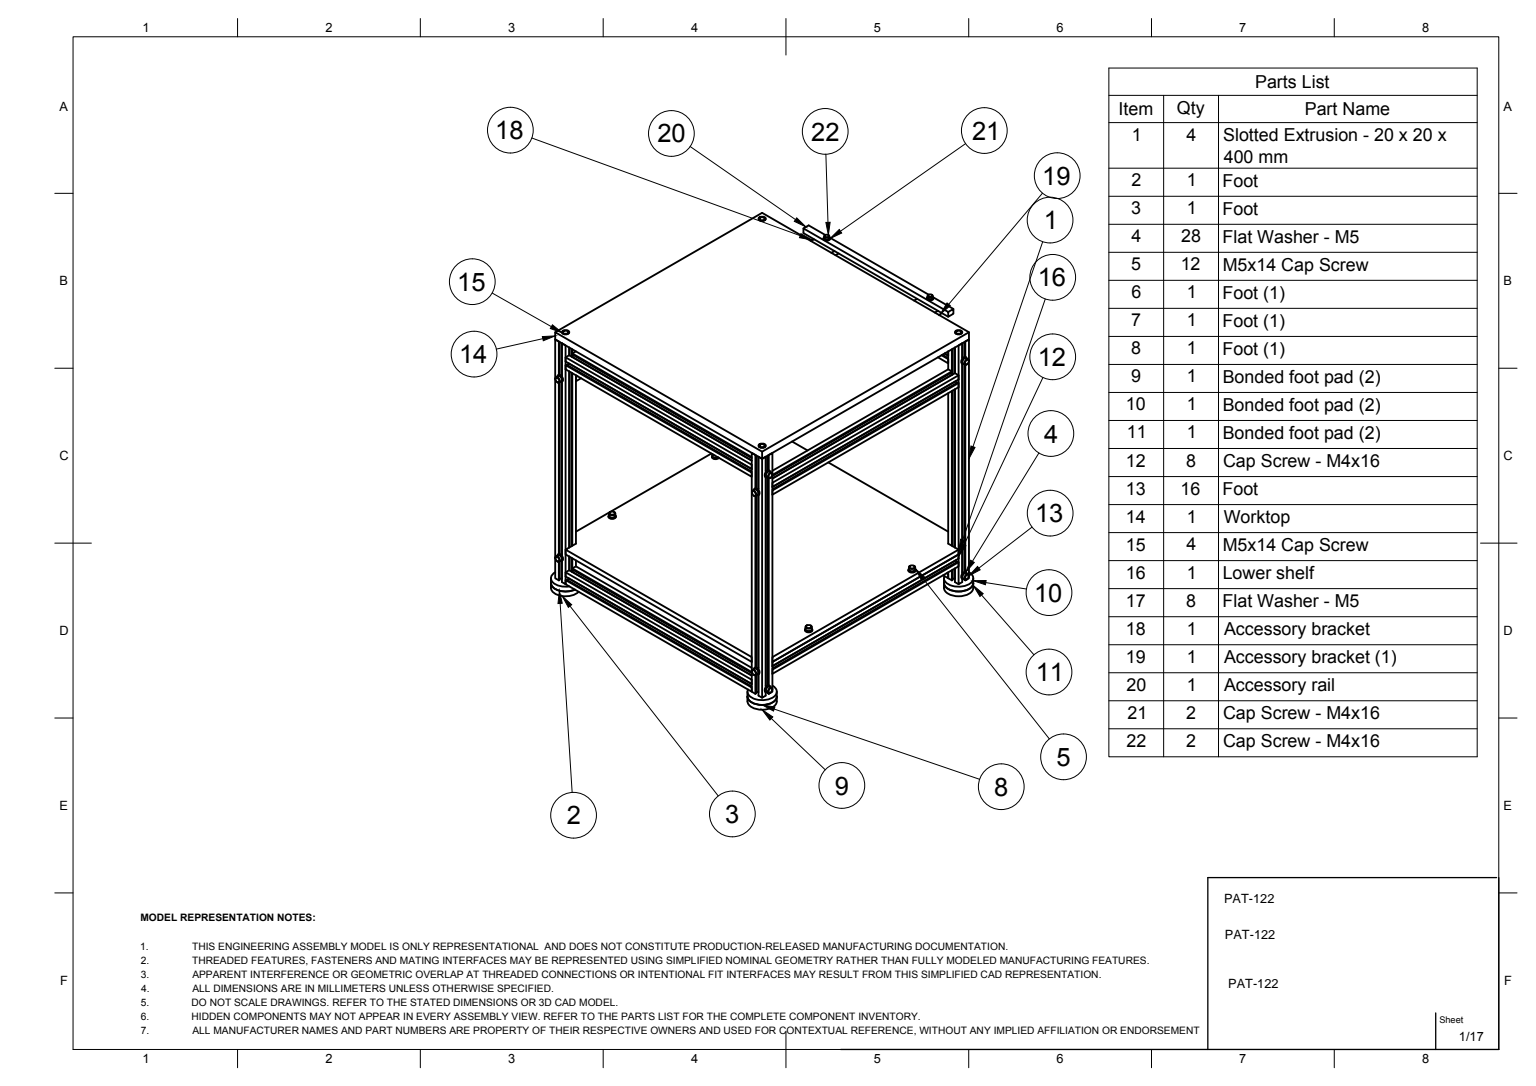
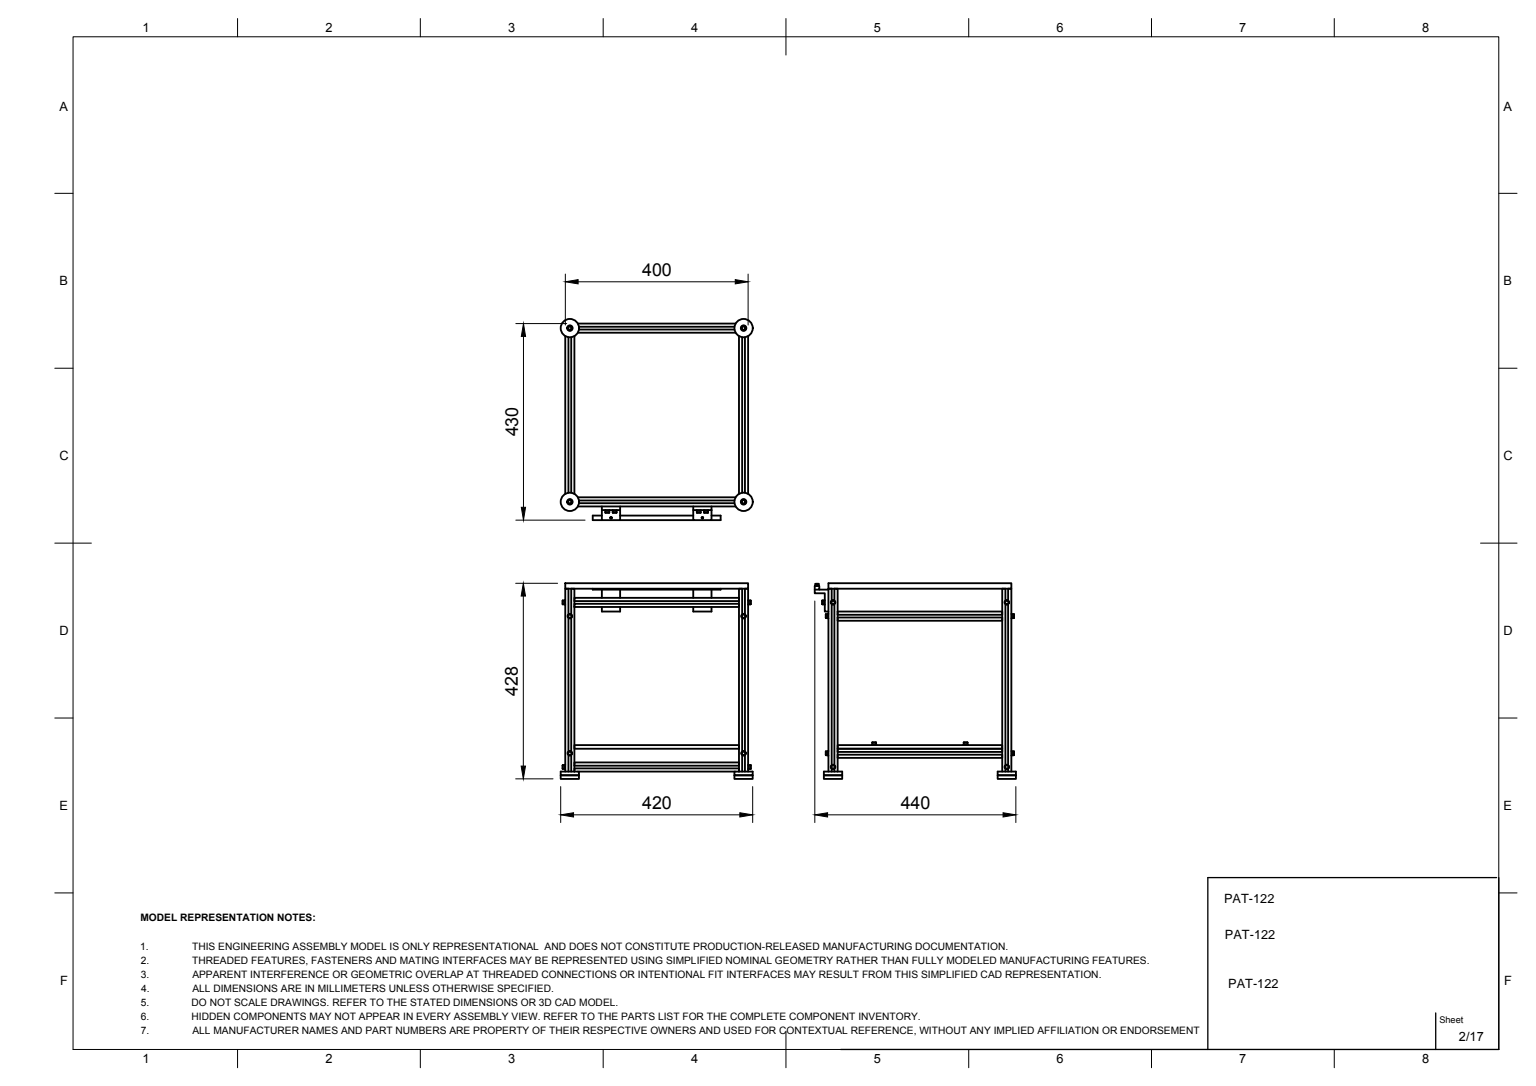
ISO-10303-21;
HEADER;
/* Generated by software containing ST-Developer
 * from STEP Tools, Inc. (www.steptools.com) 
 */

FILE_DESCRIPTION(
/* description */ ('PAT-122'),
/* implementation_level */ '2;1');

FILE_NAME(
/* name */ 'PAT-122',
/* time_stamp */ '2026-10-29T20:20:12-07:00',
/* author */ (''),
/* organization */ (''),
/* preprocessor_version */ 'ST-DEVELOPER v20.2',
/* originating_system */ 'Autodesk Translation Framework v15.17.0.0',
/* authorisation */ '');

FILE_SCHEMA (('AUTOMOTIVE_DESIGN { 1 0 10303 214 3 1 1 }'));
ENDSEC;

DATA;
#10=MECHANICAL_DESIGN_GEOMETRIC_PRESENTATION_REPRESENTATION('',(#491,#492,
#493,#494,#495,#496,#497,#498,#499,#500,#501,#502,#503,#504,#505,#506,#507,
#508,#509,#510,#511,#512),#10019);
#11=ITEM_DEFINED_TRANSFORMATION($,$,#5883,#6329);
#12=ITEM_DEFINED_TRANSFORMATION($,$,#5892,#6330);
#13=ITEM_DEFINED_TRANSFORMATION($,$,#5901,#6331);
#14=ITEM_DEFINED_TRANSFORMATION($,$,#5910,#6332);
#15=ITEM_DEFINED_TRANSFORMATION($,$,#5919,#6333);
#16=ITEM_DEFINED_TRANSFORMATION($,$,#5928,#6334);
#17=ITEM_DEFINED_TRANSFORMATION($,$,#5937,#6335);
#18=ITEM_DEFINED_TRANSFORMATION($,$,#5946,#6336);
#19=ITEM_DEFINED_TRANSFORMATION($,$,#5955,#6337);
#20=ITEM_DEFINED_TRANSFORMATION($,$,#5990,#6338);
#21=ITEM_DEFINED_TRANSFORMATION($,$,#6017,#6339);
#22=ITEM_DEFINED_TRANSFORMATION($,$,#6035,#6340);
#23=ITEM_DEFINED_TRANSFORMATION($,$,#6053,#6341);
#24=ITEM_DEFINED_TRANSFORMATION($,$,#6066,#6342);
#25=ITEM_DEFINED_TRANSFORMATION($,$,#6257,#6343);
#26=ITEM_DEFINED_TRANSFORMATION($,$,#6268,#6344);
#27=ITEM_DEFINED_TRANSFORMATION($,$,#6066,#6345);
#28=ITEM_DEFINED_TRANSFORMATION($,$,#6257,#6346);
#29=ITEM_DEFINED_TRANSFORMATION($,$,#6268,#6347);
#30=ITEM_DEFINED_TRANSFORMATION($,$,#6066,#6348);
#31=ITEM_DEFINED_TRANSFORMATION($,$,#6257,#6349);
#32=ITEM_DEFINED_TRANSFORMATION($,$,#6268,#6350);
#33=ITEM_DEFINED_TRANSFORMATION($,$,#6066,#6351);
#34=ITEM_DEFINED_TRANSFORMATION($,$,#6257,#6352);
#35=ITEM_DEFINED_TRANSFORMATION($,$,#6268,#6353);
#36=ITEM_DEFINED_TRANSFORMATION($,$,#6132,#6354);
#37=ITEM_DEFINED_TRANSFORMATION($,$,#6257,#6355);
#38=ITEM_DEFINED_TRANSFORMATION($,$,#6182,#6356);
#39=ITEM_DEFINED_TRANSFORMATION($,$,#6257,#6357);
#40=ITEM_DEFINED_TRANSFORMATION($,$,#6182,#6358);
#41=ITEM_DEFINED_TRANSFORMATION($,$,#6132,#6359);
#42=ITEM_DEFINED_TRANSFORMATION($,$,#6257,#6360);
#43=ITEM_DEFINED_TRANSFORMATION($,$,#6182,#6361);
#44=ITEM_DEFINED_TRANSFORMATION($,$,#6257,#6362);
#45=ITEM_DEFINED_TRANSFORMATION($,$,#6182,#6363);
#46=ITEM_DEFINED_TRANSFORMATION($,$,#6132,#6364);
#47=ITEM_DEFINED_TRANSFORMATION($,$,#6257,#6365);
#48=ITEM_DEFINED_TRANSFORMATION($,$,#6182,#6366);
#49=ITEM_DEFINED_TRANSFORMATION($,$,#6257,#6367);
#50=ITEM_DEFINED_TRANSFORMATION($,$,#6182,#6368);
#51=ITEM_DEFINED_TRANSFORMATION($,$,#6132,#6369);
#52=ITEM_DEFINED_TRANSFORMATION($,$,#6257,#6370);
#53=ITEM_DEFINED_TRANSFORMATION($,$,#6182,#6371);
#54=ITEM_DEFINED_TRANSFORMATION($,$,#6257,#6372);
#55=ITEM_DEFINED_TRANSFORMATION($,$,#6182,#6373);
#56=ITEM_DEFINED_TRANSFORMATION($,$,#6132,#6374);
#57=ITEM_DEFINED_TRANSFORMATION($,$,#6257,#6375);
#58=ITEM_DEFINED_TRANSFORMATION($,$,#6182,#6376);
#59=ITEM_DEFINED_TRANSFORMATION($,$,#6257,#6377);
#60=ITEM_DEFINED_TRANSFORMATION($,$,#6182,#6378);
#61=ITEM_DEFINED_TRANSFORMATION($,$,#6132,#6379);
#62=ITEM_DEFINED_TRANSFORMATION($,$,#6257,#6380);
#63=ITEM_DEFINED_TRANSFORMATION($,$,#6182,#6381);
#64=ITEM_DEFINED_TRANSFORMATION($,$,#6257,#6382);
#65=ITEM_DEFINED_TRANSFORMATION($,$,#6182,#6383);
#66=ITEM_DEFINED_TRANSFORMATION($,$,#6132,#6384);
#67=ITEM_DEFINED_TRANSFORMATION($,$,#6257,#6385);
#68=ITEM_DEFINED_TRANSFORMATION($,$,#6182,#6386);
#69=ITEM_DEFINED_TRANSFORMATION($,$,#6257,#6387);
#70=ITEM_DEFINED_TRANSFORMATION($,$,#6182,#6388);
#71=ITEM_DEFINED_TRANSFORMATION($,$,#6132,#6389);
#72=ITEM_DEFINED_TRANSFORMATION($,$,#6257,#6390);
#73=ITEM_DEFINED_TRANSFORMATION($,$,#6182,#6391);
#74=ITEM_DEFINED_TRANSFORMATION($,$,#6257,#6392);
#75=ITEM_DEFINED_TRANSFORMATION($,$,#6182,#6393);
#76=ITEM_DEFINED_TRANSFORMATION($,$,#6210,#6394);
#77=ITEM_DEFINED_TRANSFORMATION($,$,#6210,#6395);
#78=ITEM_DEFINED_TRANSFORMATION($,$,#6210,#6396);
#79=ITEM_DEFINED_TRANSFORMATION($,$,#6210,#6397);
#80=ITEM_DEFINED_TRANSFORMATION($,$,#6236,#6398);
#81=ITEM_DEFINED_TRANSFORMATION($,$,#6257,#6399);
#82=ITEM_DEFINED_TRANSFORMATION($,$,#6268,#6400);
#83=ITEM_DEFINED_TRANSFORMATION($,$,#6236,#6401);
#84=ITEM_DEFINED_TRANSFORMATION($,$,#6257,#6402);
#85=ITEM_DEFINED_TRANSFORMATION($,$,#6268,#6403);
#86=ITEM_DEFINED_TRANSFORMATION($,$,#6236,#6404);
#87=ITEM_DEFINED_TRANSFORMATION($,$,#6257,#6405);
#88=ITEM_DEFINED_TRANSFORMATION($,$,#6268,#6406);
#89=ITEM_DEFINED_TRANSFORMATION($,$,#6236,#6407);
#90=ITEM_DEFINED_TRANSFORMATION($,$,#6257,#6408);
#91=ITEM_DEFINED_TRANSFORMATION($,$,#6268,#6409);
#92=ITEM_DEFINED_TRANSFORMATION($,$,#6236,#6410);
#93=ITEM_DEFINED_TRANSFORMATION($,$,#6257,#6411);
#94=ITEM_DEFINED_TRANSFORMATION($,$,#6268,#6412);
#95=ITEM_DEFINED_TRANSFORMATION($,$,#6236,#6413);
#96=ITEM_DEFINED_TRANSFORMATION($,$,#6257,#6414);
#97=ITEM_DEFINED_TRANSFORMATION($,$,#6268,#6415);
#98=ITEM_DEFINED_TRANSFORMATION($,$,#6236,#6416);
#99=ITEM_DEFINED_TRANSFORMATION($,$,#6257,#6417);
#100=ITEM_DEFINED_TRANSFORMATION($,$,#6268,#6418);
#101=ITEM_DEFINED_TRANSFORMATION($,$,#6236,#6419);
#102=ITEM_DEFINED_TRANSFORMATION($,$,#6257,#6420);
#103=ITEM_DEFINED_TRANSFORMATION($,$,#6268,#6421);
#104=ITEM_DEFINED_TRANSFORMATION($,$,#6292,#6422);
#105=ITEM_DEFINED_TRANSFORMATION($,$,#6303,#6423);
#106=ITEM_DEFINED_TRANSFORMATION($,$,#6292,#6424);
#107=ITEM_DEFINED_TRANSFORMATION($,$,#6303,#6425);
#108=(
REPRESENTATION_RELATIONSHIP($,$,#10168,#10167)
REPRESENTATION_RELATIONSHIP_WITH_TRANSFORMATION(#11)
SHAPE_REPRESENTATION_RELATIONSHIP()
);
#109=(
REPRESENTATION_RELATIONSHIP($,$,#10169,#10167)
REPRESENTATION_RELATIONSHIP_WITH_TRANSFORMATION(#12)
SHAPE_REPRESENTATION_RELATIONSHIP()
);
#110=(
REPRESENTATION_RELATIONSHIP($,$,#10170,#10167)
REPRESENTATION_RELATIONSHIP_WITH_TRANSFORMATION(#13)
SHAPE_REPRESENTATION_RELATIONSHIP()
);
#111=(
REPRESENTATION_RELATIONSHIP($,$,#10171,#10167)
REPRESENTATION_RELATIONSHIP_WITH_TRANSFORMATION(#14)
SHAPE_REPRESENTATION_RELATIONSHIP()
);
#112=(
REPRESENTATION_RELATIONSHIP($,$,#10172,#10167)
REPRESENTATION_RELATIONSHIP_WITH_TRANSFORMATION(#15)
SHAPE_REPRESENTATION_RELATIONSHIP()
);
#113=(
REPRESENTATION_RELATIONSHIP($,$,#10173,#10167)
REPRESENTATION_RELATIONSHIP_WITH_TRANSFORMATION(#16)
SHAPE_REPRESENTATION_RELATIONSHIP()
);
#114=(
REPRESENTATION_RELATIONSHIP($,$,#10174,#10167)
REPRESENTATION_RELATIONSHIP_WITH_TRANSFORMATION(#17)
SHAPE_REPRESENTATION_RELATIONSHIP()
);
#115=(
REPRESENTATION_RELATIONSHIP($,$,#10175,#10167)
REPRESENTATION_RELATIONSHIP_WITH_TRANSFORMATION(#18)
SHAPE_REPRESENTATION_RELATIONSHIP()
);
#116=(
REPRESENTATION_RELATIONSHIP($,$,#10176,#10167)
REPRESENTATION_RELATIONSHIP_WITH_TRANSFORMATION(#19)
SHAPE_REPRESENTATION_RELATIONSHIP()
);
#117=(
REPRESENTATION_RELATIONSHIP($,$,#10177,#10167)
REPRESENTATION_RELATIONSHIP_WITH_TRANSFORMATION(#20)
SHAPE_REPRESENTATION_RELATIONSHIP()
);
#118=(
REPRESENTATION_RELATIONSHIP($,$,#10178,#10167)
REPRESENTATION_RELATIONSHIP_WITH_TRANSFORMATION(#21)
SHAPE_REPRESENTATION_RELATIONSHIP()
);
#119=(
REPRESENTATION_RELATIONSHIP($,$,#10179,#10167)
REPRESENTATION_RELATIONSHIP_WITH_TRANSFORMATION(#22)
SHAPE_REPRESENTATION_RELATIONSHIP()
);
#120=(
REPRESENTATION_RELATIONSHIP($,$,#10180,#10167)
REPRESENTATION_RELATIONSHIP_WITH_TRANSFORMATION(#23)
SHAPE_REPRESENTATION_RELATIONSHIP()
);
#121=(
REPRESENTATION_RELATIONSHIP($,$,#10181,#10167)
REPRESENTATION_RELATIONSHIP_WITH_TRANSFORMATION(#24)
SHAPE_REPRESENTATION_RELATIONSHIP()
);
#122=(
REPRESENTATION_RELATIONSHIP($,$,#10186,#10167)
REPRESENTATION_RELATIONSHIP_WITH_TRANSFORMATION(#25)
SHAPE_REPRESENTATION_RELATIONSHIP()
);
#123=(
REPRESENTATION_RELATIONSHIP($,$,#10187,#10167)
REPRESENTATION_RELATIONSHIP_WITH_TRANSFORMATION(#26)
SHAPE_REPRESENTATION_RELATIONSHIP()
);
#124=(
REPRESENTATION_RELATIONSHIP($,$,#10181,#10167)
REPRESENTATION_RELATIONSHIP_WITH_TRANSFORMATION(#27)
SHAPE_REPRESENTATION_RELATIONSHIP()
);
#125=(
REPRESENTATION_RELATIONSHIP($,$,#10186,#10167)
REPRESENTATION_RELATIONSHIP_WITH_TRANSFORMATION(#28)
SHAPE_REPRESENTATION_RELATIONSHIP()
);
#126=(
REPRESENTATION_RELATIONSHIP($,$,#10187,#10167)
REPRESENTATION_RELATIONSHIP_WITH_TRANSFORMATION(#29)
SHAPE_REPRESENTATION_RELATIONSHIP()
);
#127=(
REPRESENTATION_RELATIONSHIP($,$,#10181,#10167)
REPRESENTATION_RELATIONSHIP_WITH_TRANSFORMATION(#30)
SHAPE_REPRESENTATION_RELATIONSHIP()
);
#128=(
REPRESENTATION_RELATIONSHIP($,$,#10186,#10167)
REPRESENTATION_RELATIONSHIP_WITH_TRANSFORMATION(#31)
SHAPE_REPRESENTATION_RELATIONSHIP()
);
#129=(
REPRESENTATION_RELATIONSHIP($,$,#10187,#10167)
REPRESENTATION_RELATIONSHIP_WITH_TRANSFORMATION(#32)
SHAPE_REPRESENTATION_RELATIONSHIP()
);
#130=(
REPRESENTATION_RELATIONSHIP($,$,#10181,#10167)
REPRESENTATION_RELATIONSHIP_WITH_TRANSFORMATION(#33)
SHAPE_REPRESENTATION_RELATIONSHIP()
);
#131=(
REPRESENTATION_RELATIONSHIP($,$,#10186,#10167)
REPRESENTATION_RELATIONSHIP_WITH_TRANSFORMATION(#34)
SHAPE_REPRESENTATION_RELATIONSHIP()
);
#132=(
REPRESENTATION_RELATIONSHIP($,$,#10187,#10167)
REPRESENTATION_RELATIONSHIP_WITH_TRANSFORMATION(#35)
SHAPE_REPRESENTATION_RELATIONSHIP()
);
#133=(
REPRESENTATION_RELATIONSHIP($,$,#10182,#10167)
REPRESENTATION_RELATIONSHIP_WITH_TRANSFORMATION(#36)
SHAPE_REPRESENTATION_RELATIONSHIP()
);
#134=(
REPRESENTATION_RELATIONSHIP($,$,#10186,#10167)
REPRESENTATION_RELATIONSHIP_WITH_TRANSFORMATION(#37)
SHAPE_REPRESENTATION_RELATIONSHIP()
);
#135=(
REPRESENTATION_RELATIONSHIP($,$,#10183,#10167)
REPRESENTATION_RELATIONSHIP_WITH_TRANSFORMATION(#38)
SHAPE_REPRESENTATION_RELATIONSHIP()
);
#136=(
REPRESENTATION_RELATIONSHIP($,$,#10186,#10167)
REPRESENTATION_RELATIONSHIP_WITH_TRANSFORMATION(#39)
SHAPE_REPRESENTATION_RELATIONSHIP()
);
#137=(
REPRESENTATION_RELATIONSHIP($,$,#10183,#10167)
REPRESENTATION_RELATIONSHIP_WITH_TRANSFORMATION(#40)
SHAPE_REPRESENTATION_RELATIONSHIP()
);
#138=(
REPRESENTATION_RELATIONSHIP($,$,#10182,#10167)
REPRESENTATION_RELATIONSHIP_WITH_TRANSFORMATION(#41)
SHAPE_REPRESENTATION_RELATIONSHIP()
);
#139=(
REPRESENTATION_RELATIONSHIP($,$,#10186,#10167)
REPRESENTATION_RELATIONSHIP_WITH_TRANSFORMATION(#42)
SHAPE_REPRESENTATION_RELATIONSHIP()
);
#140=(
REPRESENTATION_RELATIONSHIP($,$,#10183,#10167)
REPRESENTATION_RELATIONSHIP_WITH_TRANSFORMATION(#43)
SHAPE_REPRESENTATION_RELATIONSHIP()
);
#141=(
REPRESENTATION_RELATIONSHIP($,$,#10186,#10167)
REPRESENTATION_RELATIONSHIP_WITH_TRANSFORMATION(#44)
SHAPE_REPRESENTATION_RELATIONSHIP()
);
#142=(
REPRESENTATION_RELATIONSHIP($,$,#10183,#10167)
REPRESENTATION_RELATIONSHIP_WITH_TRANSFORMATION(#45)
SHAPE_REPRESENTATION_RELATIONSHIP()
);
#143=(
REPRESENTATION_RELATIONSHIP($,$,#10182,#10167)
REPRESENTATION_RELATIONSHIP_WITH_TRANSFORMATION(#46)
SHAPE_REPRESENTATION_RELATIONSHIP()
);
#144=(
REPRESENTATION_RELATIONSHIP($,$,#10186,#10167)
REPRESENTATION_RELATIONSHIP_WITH_TRANSFORMATION(#47)
SHAPE_REPRESENTATION_RELATIONSHIP()
);
#145=(
REPRESENTATION_RELATIONSHIP($,$,#10183,#10167)
REPRESENTATION_RELATIONSHIP_WITH_TRANSFORMATION(#48)
SHAPE_REPRESENTATION_RELATIONSHIP()
);
#146=(
REPRESENTATION_RELATIONSHIP($,$,#10186,#10167)
REPRESENTATION_RELATIONSHIP_WITH_TRANSFORMATION(#49)
SHAPE_REPRESENTATION_RELATIONSHIP()
);
#147=(
REPRESENTATION_RELATIONSHIP($,$,#10183,#10167)
REPRESENTATION_RELATIONSHIP_WITH_TRANSFORMATION(#50)
SHAPE_REPRESENTATION_RELATIONSHIP()
);
#148=(
REPRESENTATION_RELATIONSHIP($,$,#10182,#10167)
REPRESENTATION_RELATIONSHIP_WITH_TRANSFORMATION(#51)
SHAPE_REPRESENTATION_RELATIONSHIP()
);
#149=(
REPRESENTATION_RELATIONSHIP($,$,#10186,#10167)
REPRESENTATION_RELATIONSHIP_WITH_TRANSFORMATION(#52)
SHAPE_REPRESENTATION_RELATIONSHIP()
);
#150=(
REPRESENTATION_RELATIONSHIP($,$,#10183,#10167)
REPRESENTATION_RELATIONSHIP_WITH_TRANSFORMATION(#53)
SHAPE_REPRESENTATION_RELATIONSHIP()
);
#151=(
REPRESENTATION_RELATIONSHIP($,$,#10186,#10167)
REPRESENTATION_RELATIONSHIP_WITH_TRANSFORMATION(#54)
SHAPE_REPRESENTATION_RELATIONSHIP()
);
#152=(
REPRESENTATION_RELATIONSHIP($,$,#10183,#10167)
REPRESENTATION_RELATIONSHIP_WITH_TRANSFORMATION(#55)
SHAPE_REPRESENTATION_RELATIONSHIP()
);
#153=(
REPRESENTATION_RELATIONSHIP($,$,#10182,#10167)
REPRESENTATION_RELATIONSHIP_WITH_TRANSFORMATION(#56)
SHAPE_REPRESENTATION_RELATIONSHIP()
);
#154=(
REPRESENTATION_RELATIONSHIP($,$,#10186,#10167)
REPRESENTATION_RELATIONSHIP_WITH_TRANSFORMATION(#57)
SHAPE_REPRESENTATION_RELATIONSHIP()
);
#155=(
REPRESENTATION_RELATIONSHIP($,$,#10183,#10167)
REPRESENTATION_RELATIONSHIP_WITH_TRANSFORMATION(#58)
SHAPE_REPRESENTATION_RELATIONSHIP()
);
#156=(
REPRESENTATION_RELATIONSHIP($,$,#10186,#10167)
REPRESENTATION_RELATIONSHIP_WITH_TRANSFORMATION(#59)
SHAPE_REPRESENTATION_RELATIONSHIP()
);
#157=(
REPRESENTATION_RELATIONSHIP($,$,#10183,#10167)
REPRESENTATION_RELATIONSHIP_WITH_TRANSFORMATION(#60)
SHAPE_REPRESENTATION_RELATIONSHIP()
);
#158=(
REPRESENTATION_RELATIONSHIP($,$,#10182,#10167)
REPRESENTATION_RELATIONSHIP_WITH_TRANSFORMATION(#61)
SHAPE_REPRESENTATION_RELATIONSHIP()
);
#159=(
REPRESENTATION_RELATIONSHIP($,$,#10186,#10167)
REPRESENTATION_RELATIONSHIP_WITH_TRANSFORMATION(#62)
SHAPE_REPRESENTATION_RELATIONSHIP()
);
#160=(
REPRESENTATION_RELATIONSHIP($,$,#10183,#10167)
REPRESENTATION_RELATIONSHIP_WITH_TRANSFORMATION(#63)
SHAPE_REPRESENTATION_RELATIONSHIP()
);
#161=(
REPRESENTATION_RELATIONSHIP($,$,#10186,#10167)
REPRESENTATION_RELATIONSHIP_WITH_TRANSFORMATION(#64)
SHAPE_REPRESENTATION_RELATIONSHIP()
);
#162=(
REPRESENTATION_RELATIONSHIP($,$,#10183,#10167)
REPRESENTATION_RELATIONSHIP_WITH_TRANSFORMATION(#65)
SHAPE_REPRESENTATION_RELATIONSHIP()
);
#163=(
REPRESENTATION_RELATIONSHIP($,$,#10182,#10167)
REPRESENTATION_RELATIONSHIP_WITH_TRANSFORMATION(#66)
SHAPE_REPRESENTATION_RELATIONSHIP()
);
#164=(
REPRESENTATION_RELATIONSHIP($,$,#10186,#10167)
REPRESENTATION_RELATIONSHIP_WITH_TRANSFORMATION(#67)
SHAPE_REPRESENTATION_RELATIONSHIP()
);
#165=(
REPRESENTATION_RELATIONSHIP($,$,#10183,#10167)
REPRESENTATION_RELATIONSHIP_WITH_TRANSFORMATION(#68)
SHAPE_REPRESENTATION_RELATIONSHIP()
);
#166=(
REPRESENTATION_RELATIONSHIP($,$,#10186,#10167)
REPRESENTATION_RELATIONSHIP_WITH_TRANSFORMATION(#69)
SHAPE_REPRESENTATION_RELATIONSHIP()
);
#167=(
REPRESENTATION_RELATIONSHIP($,$,#10183,#10167)
REPRESENTATION_RELATIONSHIP_WITH_TRANSFORMATION(#70)
SHAPE_REPRESENTATION_RELATIONSHIP()
);
#168=(
REPRESENTATION_RELATIONSHIP($,$,#10182,#10167)
REPRESENTATION_RELATIONSHIP_WITH_TRANSFORMATION(#71)
SHAPE_REPRESENTATION_RELATIONSHIP()
);
#169=(
REPRESENTATION_RELATIONSHIP($,$,#10186,#10167)
REPRESENTATION_RELATIONSHIP_WITH_TRANSFORMATION(#72)
SHAPE_REPRESENTATION_RELATIONSHIP()
);
#170=(
REPRESENTATION_RELATIONSHIP($,$,#10183,#10167)
REPRESENTATION_RELATIONSHIP_WITH_TRANSFORMATION(#73)
SHAPE_REPRESENTATION_RELATIONSHIP()
);
#171=(
REPRESENTATION_RELATIONSHIP($,$,#10186,#10167)
REPRESENTATION_RELATIONSHIP_WITH_TRANSFORMATION(#74)
SHAPE_REPRESENTATION_RELATIONSHIP()
);
#172=(
REPRESENTATION_RELATIONSHIP($,$,#10183,#10167)
REPRESENTATION_RELATIONSHIP_WITH_TRANSFORMATION(#75)
SHAPE_REPRESENTATION_RELATIONSHIP()
);
#173=(
REPRESENTATION_RELATIONSHIP($,$,#10184,#10167)
REPRESENTATION_RELATIONSHIP_WITH_TRANSFORMATION(#76)
SHAPE_REPRESENTATION_RELATIONSHIP()
);
#174=(
REPRESENTATION_RELATIONSHIP($,$,#10184,#10167)
REPRESENTATION_RELATIONSHIP_WITH_TRANSFORMATION(#77)
SHAPE_REPRESENTATION_RELATIONSHIP()
);
#175=(
REPRESENTATION_RELATIONSHIP($,$,#10184,#10167)
REPRESENTATION_RELATIONSHIP_WITH_TRANSFORMATION(#78)
SHAPE_REPRESENTATION_RELATIONSHIP()
);
#176=(
REPRESENTATION_RELATIONSHIP($,$,#10184,#10167)
REPRESENTATION_RELATIONSHIP_WITH_TRANSFORMATION(#79)
SHAPE_REPRESENTATION_RELATIONSHIP()
);
#177=(
REPRESENTATION_RELATIONSHIP($,$,#10185,#10167)
REPRESENTATION_RELATIONSHIP_WITH_TRANSFORMATION(#80)
SHAPE_REPRESENTATION_RELATIONSHIP()
);
#178=(
REPRESENTATION_RELATIONSHIP($,$,#10186,#10167)
REPRESENTATION_RELATIONSHIP_WITH_TRANSFORMATION(#81)
SHAPE_REPRESENTATION_RELATIONSHIP()
);
#179=(
REPRESENTATION_RELATIONSHIP($,$,#10187,#10167)
REPRESENTATION_RELATIONSHIP_WITH_TRANSFORMATION(#82)
SHAPE_REPRESENTATION_RELATIONSHIP()
);
#180=(
REPRESENTATION_RELATIONSHIP($,$,#10185,#10167)
REPRESENTATION_RELATIONSHIP_WITH_TRANSFORMATION(#83)
SHAPE_REPRESENTATION_RELATIONSHIP()
);
#181=(
REPRESENTATION_RELATIONSHIP($,$,#10186,#10167)
REPRESENTATION_RELATIONSHIP_WITH_TRANSFORMATION(#84)
SHAPE_REPRESENTATION_RELATIONSHIP()
);
#182=(
REPRESENTATION_RELATIONSHIP($,$,#10187,#10167)
REPRESENTATION_RELATIONSHIP_WITH_TRANSFORMATION(#85)
SHAPE_REPRESENTATION_RELATIONSHIP()
);
#183=(
REPRESENTATION_RELATIONSHIP($,$,#10185,#10167)
REPRESENTATION_RELATIONSHIP_WITH_TRANSFORMATION(#86)
SHAPE_REPRESENTATION_RELATIONSHIP()
);
#184=(
REPRESENTATION_RELATIONSHIP($,$,#10186,#10167)
REPRESENTATION_RELATIONSHIP_WITH_TRANSFORMATION(#87)
SHAPE_REPRESENTATION_RELATIONSHIP()
);
#185=(
REPRESENTATION_RELATIONSHIP($,$,#10187,#10167)
REPRESENTATION_RELATIONSHIP_WITH_TRANSFORMATION(#88)
SHAPE_REPRESENTATION_RELATIONSHIP()
);
#186=(
REPRESENTATION_RELATIONSHIP($,$,#10185,#10167)
REPRESENTATION_RELATIONSHIP_WITH_TRANSFORMATION(#89)
SHAPE_REPRESENTATION_RELATIONSHIP()
);
#187=(
REPRESENTATION_RELATIONSHIP($,$,#10186,#10167)
REPRESENTATION_RELATIONSHIP_WITH_TRANSFORMATION(#90)
SHAPE_REPRESENTATION_RELATIONSHIP()
);
#188=(
REPRESENTATION_RELATIONSHIP($,$,#10187,#10167)
REPRESENTATION_RELATIONSHIP_WITH_TRANSFORMATION(#91)
SHAPE_REPRESENTATION_RELATIONSHIP()
);
#189=(
REPRESENTATION_RELATIONSHIP($,$,#10185,#10167)
REPRESENTATION_RELATIONSHIP_WITH_TRANSFORMATION(#92)
SHAPE_REPRESENTATION_RELATIONSHIP()
);
#190=(
REPRESENTATION_RELATIONSHIP($,$,#10186,#10167)
REPRESENTATION_RELATIONSHIP_WITH_TRANSFORMATION(#93)
SHAPE_REPRESENTATION_RELATIONSHIP()
);
#191=(
REPRESENTATION_RELATIONSHIP($,$,#10187,#10167)
REPRESENTATION_RELATIONSHIP_WITH_TRANSFORMATION(#94)
SHAPE_REPRESENTATION_RELATIONSHIP()
);
#192=(
REPRESENTATION_RELATIONSHIP($,$,#10185,#10167)
REPRESENTATION_RELATIONSHIP_WITH_TRANSFORMATION(#95)
SHAPE_REPRESENTATION_RELATIONSHIP()
);
#193=(
REPRESENTATION_RELATIONSHIP($,$,#10186,#10167)
REPRESENTATION_RELATIONSHIP_WITH_TRANSFORMATION(#96)
SHAPE_REPRESENTATION_RELATIONSHIP()
);
#194=(
REPRESENTATION_RELATIONSHIP($,$,#10187,#10167)
REPRESENTATION_RELATIONSHIP_WITH_TRANSFORMATION(#97)
SHAPE_REPRESENTATION_RELATIONSHIP()
);
#195=(
REPRESENTATION_RELATIONSHIP($,$,#10185,#10167)
REPRESENTATION_RELATIONSHIP_WITH_TRANSFORMATION(#98)
SHAPE_REPRESENTATION_RELATIONSHIP()
);
#196=(
REPRESENTATION_RELATIONSHIP($,$,#10186,#10167)
REPRESENTATION_RELATIONSHIP_WITH_TRANSFORMATION(#99)
SHAPE_REPRESENTATION_RELATIONSHIP()
);
#197=(
REPRESENTATION_RELATIONSHIP($,$,#10187,#10167)
REPRESENTATION_RELATIONSHIP_WITH_TRANSFORMATION(#100)
SHAPE_REPRESENTATION_RELATIONSHIP()
);
#198=(
REPRESENTATION_RELATIONSHIP($,$,#10185,#10167)
REPRESENTATION_RELATIONSHIP_WITH_TRANSFORMATION(#101)
SHAPE_REPRESENTATION_RELATIONSHIP()
);
#199=(
REPRESENTATION_RELATIONSHIP($,$,#10186,#10167)
REPRESENTATION_RELATIONSHIP_WITH_TRANSFORMATION(#102)
SHAPE_REPRESENTATION_RELATIONSHIP()
);
#200=(
REPRESENTATION_RELATIONSHIP($,$,#10187,#10167)
REPRESENTATION_RELATIONSHIP_WITH_TRANSFORMATION(#103)
SHAPE_REPRESENTATION_RELATIONSHIP()
);
#201=(
REPRESENTATION_RELATIONSHIP($,$,#10188,#10167)
REPRESENTATION_RELATIONSHIP_WITH_TRANSFORMATION(#104)
SHAPE_REPRESENTATION_RELATIONSHIP()
);
#202=(
REPRESENTATION_RELATIONSHIP($,$,#10189,#10167)
REPRESENTATION_RELATIONSHIP_WITH_TRANSFORMATION(#105)
SHAPE_REPRESENTATION_RELATIONSHIP()
);
#203=(
REPRESENTATION_RELATIONSHIP($,$,#10188,#10167)
REPRESENTATION_RELATIONSHIP_WITH_TRANSFORMATION(#106)
SHAPE_REPRESENTATION_RELATIONSHIP()
);
#204=(
REPRESENTATION_RELATIONSHIP($,$,#10189,#10167)
REPRESENTATION_RELATIONSHIP_WITH_TRANSFORMATION(#107)
SHAPE_REPRESENTATION_RELATIONSHIP()
);
#205=CONTEXT_DEPENDENT_SHAPE_REPRESENTATION(#108,#10070);
#206=CONTEXT_DEPENDENT_SHAPE_REPRESENTATION(#109,#10071);
#207=CONTEXT_DEPENDENT_SHAPE_REPRESENTATION(#110,#10072);
#208=CONTEXT_DEPENDENT_SHAPE_REPRESENTATION(#111,#10073);
#209=CONTEXT_DEPENDENT_SHAPE_REPRESENTATION(#112,#10074);
#210=CONTEXT_DEPENDENT_SHAPE_REPRESENTATION(#113,#10075);
#211=CONTEXT_DEPENDENT_SHAPE_REPRESENTATION(#114,#10076);
#212=CONTEXT_DEPENDENT_SHAPE_REPRESENTATION(#115,#10077);
#213=CONTEXT_DEPENDENT_SHAPE_REPRESENTATION(#116,#10078);
#214=CONTEXT_DEPENDENT_SHAPE_REPRESENTATION(#117,#10079);
#215=CONTEXT_DEPENDENT_SHAPE_REPRESENTATION(#118,#10080);
#216=CONTEXT_DEPENDENT_SHAPE_REPRESENTATION(#119,#10081);
#217=CONTEXT_DEPENDENT_SHAPE_REPRESENTATION(#120,#10082);
#218=CONTEXT_DEPENDENT_SHAPE_REPRESENTATION(#121,#10083);
#219=CONTEXT_DEPENDENT_SHAPE_REPRESENTATION(#122,#10084);
#220=CONTEXT_DEPENDENT_SHAPE_REPRESENTATION(#123,#10085);
#221=CONTEXT_DEPENDENT_SHAPE_REPRESENTATION(#124,#10086);
#222=CONTEXT_DEPENDENT_SHAPE_REPRESENTATION(#125,#10087);
#223=CONTEXT_DEPENDENT_SHAPE_REPRESENTATION(#126,#10088);
#224=CONTEXT_DEPENDENT_SHAPE_REPRESENTATION(#127,#10089);
#225=CONTEXT_DEPENDENT_SHAPE_REPRESENTATION(#128,#10090);
#226=CONTEXT_DEPENDENT_SHAPE_REPRESENTATION(#129,#10091);
#227=CONTEXT_DEPENDENT_SHAPE_REPRESENTATION(#130,#10092);
#228=CONTEXT_DEPENDENT_SHAPE_REPRESENTATION(#131,#10093);
#229=CONTEXT_DEPENDENT_SHAPE_REPRESENTATION(#132,#10094);
#230=CONTEXT_DEPENDENT_SHAPE_REPRESENTATION(#133,#10095);
#231=CONTEXT_DEPENDENT_SHAPE_REPRESENTATION(#134,#10096);
#232=CONTEXT_DEPENDENT_SHAPE_REPRESENTATION(#135,#10097);
#233=CONTEXT_DEPENDENT_SHAPE_REPRESENTATION(#136,#10098);
#234=CONTEXT_DEPENDENT_SHAPE_REPRESENTATION(#137,#10099);
#235=CONTEXT_DEPENDENT_SHAPE_REPRESENTATION(#138,#10100);
#236=CONTEXT_DEPENDENT_SHAPE_REPRESENTATION(#139,#10101);
#237=CONTEXT_DEPENDENT_SHAPE_REPRESENTATION(#140,#10102);
#238=CONTEXT_DEPENDENT_SHAPE_REPRESENTATION(#141,#10103);
#239=CONTEXT_DEPENDENT_SHAPE_REPRESENTATION(#142,#10104);
#240=CONTEXT_DEPENDENT_SHAPE_REPRESENTATION(#143,#10105);
#241=CONTEXT_DEPENDENT_SHAPE_REPRESENTATION(#144,#10106);
#242=CONTEXT_DEPENDENT_SHAPE_REPRESENTATION(#145,#10107);
#243=CONTEXT_DEPENDENT_SHAPE_REPRESENTATION(#146,#10108);
#244=CONTEXT_DEPENDENT_SHAPE_REPRESENTATION(#147,#10109);
#245=CONTEXT_DEPENDENT_SHAPE_REPRESENTATION(#148,#10110);
#246=CONTEXT_DEPENDENT_SHAPE_REPRESENTATION(#149,#10111);
#247=CONTEXT_DEPENDENT_SHAPE_REPRESENTATION(#150,#10112);
#248=CONTEXT_DEPENDENT_SHAPE_REPRESENTATION(#151,#10113);
#249=CONTEXT_DEPENDENT_SHAPE_REPRESENTATION(#152,#10114);
#250=CONTEXT_DEPENDENT_SHAPE_REPRESENTATION(#153,#10115);
#251=CONTEXT_DEPENDENT_SHAPE_REPRESENTATION(#154,#10116);
#252=CONTEXT_DEPENDENT_SHAPE_REPRESENTATION(#155,#10117);
#253=CONTEXT_DEPENDENT_SHAPE_REPRESENTATION(#156,#10118);
#254=CONTEXT_DEPENDENT_SHAPE_REPRESENTATION(#157,#10119);
#255=CONTEXT_DEPENDENT_SHAPE_REPRESENTATION(#158,#10120);
#256=CONTEXT_DEPENDENT_SHAPE_REPRESENTATION(#159,#10121);
#257=CONTEXT_DEPENDENT_SHAPE_REPRESENTATION(#160,#10122);
#258=CONTEXT_DEPENDENT_SHAPE_REPRESENTATION(#161,#10123);
#259=CONTEXT_DEPENDENT_SHAPE_REPRESENTATION(#162,#10124);
#260=CONTEXT_DEPENDENT_SHAPE_REPRESENTATION(#163,#10125);
#261=CONTEXT_DEPENDENT_SHAPE_REPRESENTATION(#164,#10126);
#262=CONTEXT_DEPENDENT_SHAPE_REPRESENTATION(#165,#10127);
#263=CONTEXT_DEPENDENT_SHAPE_REPRESENTATION(#166,#10128);
#264=CONTEXT_DEPENDENT_SHAPE_REPRESENTATION(#167,#10129);
#265=CONTEXT_DEPENDENT_SHAPE_REPRESENTATION(#168,#10130);
#266=CONTEXT_DEPENDENT_SHAPE_REPRESENTATION(#169,#10131);
#267=CONTEXT_DEPENDENT_SHAPE_REPRESENTATION(#170,#10132);
#268=CONTEXT_DEPENDENT_SHAPE_REPRESENTATION(#171,#10133);
#269=CONTEXT_DEPENDENT_SHAPE_REPRESENTATION(#172,#10134);
#270=CONTEXT_DEPENDENT_SHAPE_REPRESENTATION(#173,#10135);
#271=CONTEXT_DEPENDENT_SHAPE_REPRESENTATION(#174,#10136);
#272=CONTEXT_DEPENDENT_SHAPE_REPRESENTATION(#175,#10137);
#273=CONTEXT_DEPENDENT_SHAPE_REPRESENTATION(#176,#10138);
#274=CONTEXT_DEPENDENT_SHAPE_REPRESENTATION(#177,#10139);
#275=CONTEXT_DEPENDENT_SHAPE_REPRESENTATION(#178,#10140);
#276=CONTEXT_DEPENDENT_SHAPE_REPRESENTATION(#179,#10141);
#277=CONTEXT_DEPENDENT_SHAPE_REPRESENTATION(#180,#10142);
#278=CONTEXT_DEPENDENT_SHAPE_REPRESENTATION(#181,#10143);
#279=CONTEXT_DEPENDENT_SHAPE_REPRESENTATION(#182,#10144);
#280=CONTEXT_DEPENDENT_SHAPE_REPRESENTATION(#183,#10145);
#281=CONTEXT_DEPENDENT_SHAPE_REPRESENTATION(#184,#10146);
#282=CONTEXT_DEPENDENT_SHAPE_REPRESENTATION(#185,#10147);
#283=CONTEXT_DEPENDENT_SHAPE_REPRESENTATION(#186,#10148);
#284=CONTEXT_DEPENDENT_SHAPE_REPRESENTATION(#187,#10149);
#285=CONTEXT_DEPENDENT_SHAPE_REPRESENTATION(#188,#10150);
#286=CONTEXT_DEPENDENT_SHAPE_REPRESENTATION(#189,#10151);
#287=CONTEXT_DEPENDENT_SHAPE_REPRESENTATION(#190,#10152);
#288=CONTEXT_DEPENDENT_SHAPE_REPRESENTATION(#191,#10153);
#289=CONTEXT_DEPENDENT_SHAPE_REPRESENTATION(#192,#10154);
#290=CONTEXT_DEPENDENT_SHAPE_REPRESENTATION(#193,#10155);
#291=CONTEXT_DEPENDENT_SHAPE_REPRESENTATION(#194,#10156);
#292=CONTEXT_DEPENDENT_SHAPE_REPRESENTATION(#195,#10157);
#293=CONTEXT_DEPENDENT_SHAPE_REPRESENTATION(#196,#10158);
#294=CONTEXT_DEPENDENT_SHAPE_REPRESENTATION(#197,#10159);
#295=CONTEXT_DEPENDENT_SHAPE_REPRESENTATION(#198,#10160);
#296=CONTEXT_DEPENDENT_SHAPE_REPRESENTATION(#199,#10161);
#297=CONTEXT_DEPENDENT_SHAPE_REPRESENTATION(#200,#10162);
#298=CONTEXT_DEPENDENT_SHAPE_REPRESENTATION(#201,#10163);
#299=CONTEXT_DEPENDENT_SHAPE_REPRESENTATION(#202,#10164);
#300=CONTEXT_DEPENDENT_SHAPE_REPRESENTATION(#203,#10165);
#301=CONTEXT_DEPENDENT_SHAPE_REPRESENTATION(#204,#10166);
#302=NEXT_ASSEMBLY_USAGE_OCCURRENCE('Foot:1','Foot:1','Foot:1',#10191,#10192,
'Foot:1');
#303=NEXT_ASSEMBLY_USAGE_OCCURRENCE('Bonded foot pad:1',
'Bonded foot pad:1','Bonded foot pad:1',#10191,#10193,
'Bonded foot pad:1');
#304=NEXT_ASSEMBLY_USAGE_OCCURRENCE('Foot (1):1','Foot (1):1',
'Foot (1):1',#10191,#10194,'Foot (1):1');
#305=NEXT_ASSEMBLY_USAGE_OCCURRENCE('Bonded foot pad (1):1',
'Bonded foot pad (1):1','Bonded foot pad (1):1',#10191,#10195,
'Bonded foot pad (1):1');
#306=NEXT_ASSEMBLY_USAGE_OCCURRENCE('Foot (2):1','Foot (2):1',
'Foot (2):1',#10191,#10196,'Foot (2):1');
#307=NEXT_ASSEMBLY_USAGE_OCCURRENCE('Bonded foot pad (2):1',
'Bonded foot pad (2):1','Bonded foot pad (2):1',#10191,#10197,
'Bonded foot pad (2):1');
#308=NEXT_ASSEMBLY_USAGE_OCCURRENCE('Foot (3):1','Foot (3):1',
'Foot (3):1',#10191,#10198,'Foot (3):1');
#309=NEXT_ASSEMBLY_USAGE_OCCURRENCE('Bonded foot pad (3):1',
'Bonded foot pad (3):1','Bonded foot pad (3):1',#10191,#10199,
'Bonded foot pad (3):1');
#310=NEXT_ASSEMBLY_USAGE_OCCURRENCE('Worktop:1','Worktop:1','Worktop:1',
#10191,#10200,'Worktop:1');
#311=NEXT_ASSEMBLY_USAGE_OCCURRENCE('Lower shelf:1','Lower shelf:1',
'Lower shelf:1',#10191,#10201,'Lower shelf:1');
#312=NEXT_ASSEMBLY_USAGE_OCCURRENCE('Accessory bracket:1',
'Accessory bracket:1','Accessory bracket:1',#10191,#10202,
'Accessory bracket:1');
#313=NEXT_ASSEMBLY_USAGE_OCCURRENCE('Accessory bracket (1):1',
'Accessory bracket (1):1','Accessory bracket (1):1',#10191,#10203,
'Accessory bracket (1):1');
#314=NEXT_ASSEMBLY_USAGE_OCCURRENCE('Accessory rail:1',
'Accessory rail:1','Accessory rail:1',#10191,#10204,'Accessory rail:1');
#315=NEXT_ASSEMBLY_USAGE_OCCURRENCE(
'Slotted Extrusion - 20 x 20 x 400 mm:1',
'Slotted Extrusion - 20 x 20 x 400 mm:1',
'Slotted Extrusion - 20 x 20 x 400 mm:1',#10191,#10205,
'Slotted Extrusion - 20 x 20 x 400 mm:1');
#316=NEXT_ASSEMBLY_USAGE_OCCURRENCE('Flat Washer - M5:1',
'Flat Washer - M5:1','Flat Washer - M5:1',#10191,#10210,
'Flat Washer - M5:1');
#317=NEXT_ASSEMBLY_USAGE_OCCURRENCE('M5x14 Cap Screw:1',
'M5x14 Cap Screw:1','M5x14 Cap Screw:1',#10191,#10211,
'M5x14 Cap Screw:1');
#318=NEXT_ASSEMBLY_USAGE_OCCURRENCE(
'Slotted Extrusion - 20 x 20 x 400 mm:2',
'Slotted Extrusion - 20 x 20 x 400 mm:2',
'Slotted Extrusion - 20 x 20 x 400 mm:2',#10191,#10205,
'Slotted Extrusion - 20 x 20 x 400 mm:2');
#319=NEXT_ASSEMBLY_USAGE_OCCURRENCE('Flat Washer - M5:2',
'Flat Washer - M5:2','Flat Washer - M5:2',#10191,#10210,
'Flat Washer - M5:2');
#320=NEXT_ASSEMBLY_USAGE_OCCURRENCE('M5x14 Cap Screw:2',
'M5x14 Cap Screw:2','M5x14 Cap Screw:2',#10191,#10211,
'M5x14 Cap Screw:2');
#321=NEXT_ASSEMBLY_USAGE_OCCURRENCE(
'Slotted Extrusion - 20 x 20 x 400 mm:3',
'Slotted Extrusion - 20 x 20 x 400 mm:3',
'Slotted Extrusion - 20 x 20 x 400 mm:3',#10191,#10205,
'Slotted Extrusion - 20 x 20 x 400 mm:3');
#322=NEXT_ASSEMBLY_USAGE_OCCURRENCE('Flat Washer - M5:3',
'Flat Washer - M5:3','Flat Washer - M5:3',#10191,#10210,
'Flat Washer - M5:3');
#323=NEXT_ASSEMBLY_USAGE_OCCURRENCE('M5x14 Cap Screw:3',
'M5x14 Cap Screw:3','M5x14 Cap Screw:3',#10191,#10211,
'M5x14 Cap Screw:3');
#324=NEXT_ASSEMBLY_USAGE_OCCURRENCE(
'Slotted Extrusion - 20 x 20 x 400 mm:4',
'Slotted Extrusion - 20 x 20 x 400 mm:4',
'Slotted Extrusion - 20 x 20 x 400 mm:4',#10191,#10205,
'Slotted Extrusion - 20 x 20 x 400 mm:4');
#325=NEXT_ASSEMBLY_USAGE_OCCURRENCE('Flat Washer - M5:4',
'Flat Washer - M5:4','Flat Washer - M5:4',#10191,#10210,
'Flat Washer - M5:4');
#326=NEXT_ASSEMBLY_USAGE_OCCURRENCE('M5x14 Cap Screw:4',
'M5x14 Cap Screw:4','M5x14 Cap Screw:4',#10191,#10211,
'M5x14 Cap Screw:4');
#327=NEXT_ASSEMBLY_USAGE_OCCURRENCE('360 mm cross member:1',
'360 mm cross member:1','360 mm cross member:1',#10191,#10206,
'360 mm cross member:1');
#328=NEXT_ASSEMBLY_USAGE_OCCURRENCE('Flat Washer - M5:5',
'Flat Washer - M5:5','Flat Washer - M5:5',#10191,#10210,
'Flat Washer - M5:5');
#329=NEXT_ASSEMBLY_USAGE_OCCURRENCE('M5x30 frame screw:1',
'M5x30 frame screw:1','M5x30 frame screw:1',#10191,#10207,
'M5x30 frame screw:1');
#330=NEXT_ASSEMBLY_USAGE_OCCURRENCE('Flat Washer - M5:6',
'Flat Washer - M5:6','Flat Washer - M5:6',#10191,#10210,
'Flat Washer - M5:6');
#331=NEXT_ASSEMBLY_USAGE_OCCURRENCE('M5x30 frame screw:2',
'M5x30 frame screw:2','M5x30 frame screw:2',#10191,#10207,
'M5x30 frame screw:2');
#332=NEXT_ASSEMBLY_USAGE_OCCURRENCE('360 mm cross member:2',
'360 mm cross member:2','360 mm cross member:2',#10191,#10206,
'360 mm cross member:2');
#333=NEXT_ASSEMBLY_USAGE_OCCURRENCE('Flat Washer - M5:7',
'Flat Washer - M5:7','Flat Washer - M5:7',#10191,#10210,
'Flat Washer - M5:7');
#334=NEXT_ASSEMBLY_USAGE_OCCURRENCE('M5x30 frame screw:3',
'M5x30 frame screw:3','M5x30 frame screw:3',#10191,#10207,
'M5x30 frame screw:3');
#335=NEXT_ASSEMBLY_USAGE_OCCURRENCE('Flat Washer - M5:8',
'Flat Washer - M5:8','Flat Washer - M5:8',#10191,#10210,
'Flat Washer - M5:8');
#336=NEXT_ASSEMBLY_USAGE_OCCURRENCE('M5x30 frame screw:4',
'M5x30 frame screw:4','M5x30 frame screw:4',#10191,#10207,
'M5x30 frame screw:4');
#337=NEXT_ASSEMBLY_USAGE_OCCURRENCE('360 mm cross member:3',
'360 mm cross member:3','360 mm cross member:3',#10191,#10206,
'360 mm cross member:3');
#338=NEXT_ASSEMBLY_USAGE_OCCURRENCE('Flat Washer - M5:9',
'Flat Washer - M5:9','Flat Washer - M5:9',#10191,#10210,
'Flat Washer - M5:9');
#339=NEXT_ASSEMBLY_USAGE_OCCURRENCE('M5x30 frame screw:5',
'M5x30 frame screw:5','M5x30 frame screw:5',#10191,#10207,
'M5x30 frame screw:5');
#340=NEXT_ASSEMBLY_USAGE_OCCURRENCE('Flat Washer - M5:10',
'Flat Washer - M5:10','Flat Washer - M5:10',#10191,#10210,
'Flat Washer - M5:10');
#341=NEXT_ASSEMBLY_USAGE_OCCURRENCE('M5x30 frame screw:6',
'M5x30 frame screw:6','M5x30 frame screw:6',#10191,#10207,
'M5x30 frame screw:6');
#342=NEXT_ASSEMBLY_USAGE_OCCURRENCE('360 mm cross member:4',
'360 mm cross member:4','360 mm cross member:4',#10191,#10206,
'360 mm cross member:4');
#343=NEXT_ASSEMBLY_USAGE_OCCURRENCE('Flat Washer - M5:11',
'Flat Washer - M5:11','Flat Washer - M5:11',#10191,#10210,
'Flat Washer - M5:11');
#344=NEXT_ASSEMBLY_USAGE_OCCURRENCE('M5x30 frame screw:7',
'M5x30 frame screw:7','M5x30 frame screw:7',#10191,#10207,
'M5x30 frame screw:7');
#345=NEXT_ASSEMBLY_USAGE_OCCURRENCE('Flat Washer - M5:12',
'Flat Washer - M5:12','Flat Washer - M5:12',#10191,#10210,
'Flat Washer - M5:12');
#346=NEXT_ASSEMBLY_USAGE_OCCURRENCE('M5x30 frame screw:8',
'M5x30 frame screw:8','M5x30 frame screw:8',#10191,#10207,
'M5x30 frame screw:8');
#347=NEXT_ASSEMBLY_USAGE_OCCURRENCE('360 mm cross member:5',
'360 mm cross member:5','360 mm cross member:5',#10191,#10206,
'360 mm cross member:5');
#348=NEXT_ASSEMBLY_USAGE_OCCURRENCE('Flat Washer - M5:13',
'Flat Washer - M5:13','Flat Washer - M5:13',#10191,#10210,
'Flat Washer - M5:13');
#349=NEXT_ASSEMBLY_USAGE_OCCURRENCE('M5x30 frame screw:9',
'M5x30 frame screw:9','M5x30 frame screw:9',#10191,#10207,
'M5x30 frame screw:9');
#350=NEXT_ASSEMBLY_USAGE_OCCURRENCE('Flat Washer - M5:14',
'Flat Washer - M5:14','Flat Washer - M5:14',#10191,#10210,
'Flat Washer - M5:14');
#351=NEXT_ASSEMBLY_USAGE_OCCURRENCE('M5x30 frame screw:10',
'M5x30 frame screw:10','M5x30 frame screw:10',#10191,#10207,
'M5x30 frame screw:10');
#352=NEXT_ASSEMBLY_USAGE_OCCURRENCE('360 mm cross member:6',
'360 mm cross member:6','360 mm cross member:6',#10191,#10206,
'360 mm cross member:6');
#353=NEXT_ASSEMBLY_USAGE_OCCURRENCE('Flat Washer - M5:15',
'Flat Washer - M5:15','Flat Washer - M5:15',#10191,#10210,
'Flat Washer - M5:15');
#354=NEXT_ASSEMBLY_USAGE_OCCURRENCE('M5x30 frame screw:11',
'M5x30 frame screw:11','M5x30 frame screw:11',#10191,#10207,
'M5x30 frame screw:11');
#355=NEXT_ASSEMBLY_USAGE_OCCURRENCE('Flat Washer - M5:16',
'Flat Washer - M5:16','Flat Washer - M5:16',#10191,#10210,
'Flat Washer - M5:16');
#356=NEXT_ASSEMBLY_USAGE_OCCURRENCE('M5x30 frame screw:12',
'M5x30 frame screw:12','M5x30 frame screw:12',#10191,#10207,
'M5x30 frame screw:12');
#357=NEXT_ASSEMBLY_USAGE_OCCURRENCE('360 mm cross member:7',
'360 mm cross member:7','360 mm cross member:7',#10191,#10206,
'360 mm cross member:7');
#358=NEXT_ASSEMBLY_USAGE_OCCURRENCE('Flat Washer - M5:17',
'Flat Washer - M5:17','Flat Washer - M5:17',#10191,#10210,
'Flat Washer - M5:17');
#359=NEXT_ASSEMBLY_USAGE_OCCURRENCE('M5x30 frame screw:13',
'M5x30 frame screw:13','M5x30 frame screw:13',#10191,#10207,
'M5x30 frame screw:13');
#360=NEXT_ASSEMBLY_USAGE_OCCURRENCE('Flat Washer - M5:18',
'Flat Washer - M5:18','Flat Washer - M5:18',#10191,#10210,
'Flat Washer - M5:18');
#361=NEXT_ASSEMBLY_USAGE_OCCURRENCE('M5x30 frame screw:14',
'M5x30 frame screw:14','M5x30 frame screw:14',#10191,#10207,
'M5x30 frame screw:14');
#362=NEXT_ASSEMBLY_USAGE_OCCURRENCE('360 mm cross member:8',
'360 mm cross member:8','360 mm cross member:8',#10191,#10206,
'360 mm cross member:8');
#363=NEXT_ASSEMBLY_USAGE_OCCURRENCE('Flat Washer - M5:19',
'Flat Washer - M5:19','Flat Washer - M5:19',#10191,#10210,
'Flat Washer - M5:19');
#364=NEXT_ASSEMBLY_USAGE_OCCURRENCE('M5x30 frame screw:15',
'M5x30 frame screw:15','M5x30 frame screw:15',#10191,#10207,
'M5x30 frame screw:15');
#365=NEXT_ASSEMBLY_USAGE_OCCURRENCE('Flat Washer - M5:20',
'Flat Washer - M5:20','Flat Washer - M5:20',#10191,#10210,
'Flat Washer - M5:20');
#366=NEXT_ASSEMBLY_USAGE_OCCURRENCE('M5x30 frame screw:16',
'M5x30 frame screw:16','M5x30 frame screw:16',#10191,#10207,
'M5x30 frame screw:16');
#367=NEXT_ASSEMBLY_USAGE_OCCURRENCE('Cap Screw - M5x20:1',
'Cap Screw - M5x20:1','Cap Screw - M5x20:1',#10191,#10208,
'Cap Screw - M5x20:1');
#368=NEXT_ASSEMBLY_USAGE_OCCURRENCE('Cap Screw - M5x20:2',
'Cap Screw - M5x20:2','Cap Screw - M5x20:2',#10191,#10208,
'Cap Screw - M5x20:2');
#369=NEXT_ASSEMBLY_USAGE_OCCURRENCE('Cap Screw - M5x20:3',
'Cap Screw - M5x20:3','Cap Screw - M5x20:3',#10191,#10208,
'Cap Screw - M5x20:3');
#370=NEXT_ASSEMBLY_USAGE_OCCURRENCE('Cap Screw - M5x20:4',
'Cap Screw - M5x20:4','Cap Screw - M5x20:4',#10191,#10208,
'Cap Screw - M5x20:4');
#371=NEXT_ASSEMBLY_USAGE_OCCURRENCE('Captive slot nut:1',
'Captive slot nut:1','Captive slot nut:1',#10191,#10209,
'Captive slot nut:1');
#372=NEXT_ASSEMBLY_USAGE_OCCURRENCE('Flat Washer - M5:21',
'Flat Washer - M5:21','Flat Washer - M5:21',#10191,#10210,
'Flat Washer - M5:21');
#373=NEXT_ASSEMBLY_USAGE_OCCURRENCE('M5x14 Cap Screw:5',
'M5x14 Cap Screw:5','M5x14 Cap Screw:5',#10191,#10211,
'M5x14 Cap Screw:5');
#374=NEXT_ASSEMBLY_USAGE_OCCURRENCE('Captive slot nut:2',
'Captive slot nut:2','Captive slot nut:2',#10191,#10209,
'Captive slot nut:2');
#375=NEXT_ASSEMBLY_USAGE_OCCURRENCE('Flat Washer - M5:22',
'Flat Washer - M5:22','Flat Washer - M5:22',#10191,#10210,
'Flat Washer - M5:22');
#376=NEXT_ASSEMBLY_USAGE_OCCURRENCE('M5x14 Cap Screw:6',
'M5x14 Cap Screw:6','M5x14 Cap Screw:6',#10191,#10211,
'M5x14 Cap Screw:6');
#377=NEXT_ASSEMBLY_USAGE_OCCURRENCE('Captive slot nut:3',
'Captive slot nut:3','Captive slot nut:3',#10191,#10209,
'Captive slot nut:3');
#378=NEXT_ASSEMBLY_USAGE_OCCURRENCE('Flat Washer - M5:23',
'Flat Washer - M5:23','Flat Washer - M5:23',#10191,#10210,
'Flat Washer - M5:23');
#379=NEXT_ASSEMBLY_USAGE_OCCURRENCE('M5x14 Cap Screw:7',
'M5x14 Cap Screw:7','M5x14 Cap Screw:7',#10191,#10211,
'M5x14 Cap Screw:7');
#380=NEXT_ASSEMBLY_USAGE_OCCURRENCE('Captive slot nut:4',
'Captive slot nut:4','Captive slot nut:4',#10191,#10209,
'Captive slot nut:4');
#381=NEXT_ASSEMBLY_USAGE_OCCURRENCE('Flat Washer - M5:24',
'Flat Washer - M5:24','Flat Washer - M5:24',#10191,#10210,
'Flat Washer - M5:24');
#382=NEXT_ASSEMBLY_USAGE_OCCURRENCE('M5x14 Cap Screw:8',
'M5x14 Cap Screw:8','M5x14 Cap Screw:8',#10191,#10211,
'M5x14 Cap Screw:8');
#383=NEXT_ASSEMBLY_USAGE_OCCURRENCE('Captive slot nut:5',
'Captive slot nut:5','Captive slot nut:5',#10191,#10209,
'Captive slot nut:5');
#384=NEXT_ASSEMBLY_USAGE_OCCURRENCE('Flat Washer - M5:25',
'Flat Washer - M5:25','Flat Washer - M5:25',#10191,#10210,
'Flat Washer - M5:25');
#385=NEXT_ASSEMBLY_USAGE_OCCURRENCE('M5x14 Cap Screw:9',
'M5x14 Cap Screw:9','M5x14 Cap Screw:9',#10191,#10211,
'M5x14 Cap Screw:9');
#386=NEXT_ASSEMBLY_USAGE_OCCURRENCE('Captive slot nut:6',
'Captive slot nut:6','Captive slot nut:6',#10191,#10209,
'Captive slot nut:6');
#387=NEXT_ASSEMBLY_USAGE_OCCURRENCE('Flat Washer - M5:26',
'Flat Washer - M5:26','Flat Washer - M5:26',#10191,#10210,
'Flat Washer - M5:26');
#388=NEXT_ASSEMBLY_USAGE_OCCURRENCE('M5x14 Cap Screw:10',
'M5x14 Cap Screw:10','M5x14 Cap Screw:10',#10191,#10211,
'M5x14 Cap Screw:10');
#389=NEXT_ASSEMBLY_USAGE_OCCURRENCE('Captive slot nut:7',
'Captive slot nut:7','Captive slot nut:7',#10191,#10209,
'Captive slot nut:7');
#390=NEXT_ASSEMBLY_USAGE_OCCURRENCE('Flat Washer - M5:27',
'Flat Washer - M5:27','Flat Washer - M5:27',#10191,#10210,
'Flat Washer - M5:27');
#391=NEXT_ASSEMBLY_USAGE_OCCURRENCE('M5x14 Cap Screw:11',
'M5x14 Cap Screw:11','M5x14 Cap Screw:11',#10191,#10211,
'M5x14 Cap Screw:11');
#392=NEXT_ASSEMBLY_USAGE_OCCURRENCE('Captive slot nut:8',
'Captive slot nut:8','Captive slot nut:8',#10191,#10209,
'Captive slot nut:8');
#393=NEXT_ASSEMBLY_USAGE_OCCURRENCE('Flat Washer - M5:28',
'Flat Washer - M5:28','Flat Washer - M5:28',#10191,#10210,
'Flat Washer - M5:28');
#394=NEXT_ASSEMBLY_USAGE_OCCURRENCE('M5x14 Cap Screw:12',
'M5x14 Cap Screw:12','M5x14 Cap Screw:12',#10191,#10211,
'M5x14 Cap Screw:12');
#395=NEXT_ASSEMBLY_USAGE_OCCURRENCE('Flat Washer - M4:1',
'Flat Washer - M4:1','Flat Washer - M4:1',#10191,#10212,
'Flat Washer - M4:1');
#396=NEXT_ASSEMBLY_USAGE_OCCURRENCE('Cap Screw - M4x16:1',
'Cap Screw - M4x16:1','Cap Screw - M4x16:1',#10191,#10213,
'Cap Screw - M4x16:1');
#397=NEXT_ASSEMBLY_USAGE_OCCURRENCE('Flat Washer - M4:2',
'Flat Washer - M4:2','Flat Washer - M4:2',#10191,#10212,
'Flat Washer - M4:2');
#398=NEXT_ASSEMBLY_USAGE_OCCURRENCE('Cap Screw - M4x16:2',
'Cap Screw - M4x16:2','Cap Screw - M4x16:2',#10191,#10213,
'Cap Screw - M4x16:2');
#399=ELLIPSE('',#6247,0.299389011154384,0.2117);
#400=ELLIPSE('',#6251,0.299389011154384,0.2117);
#401=CONICAL_SURFACE('',#6199,0.4,0.785398163397448);
#402=CONICAL_SURFACE('',#6203,0.41,0.785398163397448);
#403=CONICAL_SURFACE('',#6207,0.26,0.463647609000806);
#404=CONICAL_SURFACE('',#6213,0.4,0.785398163397448);
#405=CONICAL_SURFACE('',#6217,0.41,0.785398163397448);
#406=CONICAL_SURFACE('',#6221,0.26,0.463647609000806);
#407=CONICAL_SURFACE('',#6225,0.225,0.785398163397448);
#408=CONICAL_SURFACE('',#6258,0.275,0.785398163397449);
#409=CONICAL_SURFACE('',#6281,0.4,0.785398163397448);
#410=CONICAL_SURFACE('',#6285,0.41,0.785398163397448);
#411=CONICAL_SURFACE('',#6289,0.26,0.463647609000806);
#412=CONICAL_SURFACE('',#6293,0.225,0.785398163397448);
#413=CONICAL_SURFACE('',#6306,0.325,0.785398163397448);
#414=CONICAL_SURFACE('',#6310,0.335,0.785398163397448);
#415=CONICAL_SURFACE('',#6314,0.21,0.463647609000806);
#416=CONICAL_SURFACE('',#6318,0.18,0.785398163397448);
#417=ORIENTED_CLOSED_SHELL('',*,#5628,.F.);
#418=ORIENTED_CLOSED_SHELL('',*,#5631,.F.);
#419=ORIENTED_CLOSED_SHELL('',*,#5634,.F.);
#420=ORIENTED_CLOSED_SHELL('',*,#5638,.F.);
#421=BREP_WITH_VOIDS('Body1',#5629,(#417));
#422=BREP_WITH_VOIDS('Body1',#5630,(#418));
#423=BREP_WITH_VOIDS('Body1',#5635,(#419));
#424=BREP_WITH_VOIDS('Body1',#5637,(#420));
#425=B_SPLINE_CURVE_WITH_KNOTS('',3,(#8517,#8518,#8519,#8520,#8521,#8522,
#8523,#8524,#8525,#8526,#8527,#8528),.UNSPECIFIED.,.F.,.F.,(4,2,2,2,2,4),
(0.671876099962389,0.714365153473771,0.756854206985153,0.841832314007917,
0.92482323197575,1.00781414994358),.UNSPECIFIED.);
#426=B_SPLINE_CURVE_WITH_KNOTS('',3,(#8530,#8531,#8532,#8533,#8534,#8535,
#8536,#8537,#8538,#8539,#8540,#8541),.UNSPECIFIED.,.F.,.F.,(4,2,2,2,2,4),
(0.335938049981194,0.418928967949028,0.501919885916861,0.586897992939625,
0.629387046451007,0.671876099962389),.UNSPECIFIED.);
#427=B_SPLINE_CURVE_WITH_KNOTS('',3,(#8546,#8547,#8548,#8549,#8550,#8551,
#8552,#8553,#8554,#8555,#8556,#8557),.UNSPECIFIED.,.F.,.F.,(4,2,2,2,2,4),
(0.,0.042489053511382,0.0849781070227641,0.169956214045528,0.252947132013361,
0.335938049981194),.UNSPECIFIED.);
#428=B_SPLINE_CURVE_WITH_KNOTS('',3,(#8558,#8559,#8560,#8561,#8562,#8563,
#8564,#8565,#8566,#8567,#8568,#8569),.UNSPECIFIED.,.F.,.F.,(4,2,2,2,2,4),
(1.00781414994358,1.09080506791142,1.17379598587925,1.25877409290201,1.3012631464134,
1.34375219992478),.UNSPECIFIED.);
#429=B_SPLINE_CURVE_WITH_KNOTS('',3,(#8572,#8573,#8574,#8575,#8576,#8577,
#8578,#8579,#8580,#8581,#8582,#8583,#8584,#8585,#8586,#8587,#8588,#8589,
#8590,#8591,#8592,#8593),.UNSPECIFIED.,.F.,.F.,(4,2,2,2,2,2,2,2,2,2,4),
(0.,0.0424890535113821,0.0849781070227642,0.169956214045528,0.252947132013361,
0.335938049981194,0.418928967949028,0.501919885916861,0.586897992939625,
0.629387046451007,0.671876099962389),.UNSPECIFIED.);
#430=B_SPLINE_CURVE_WITH_KNOTS('',3,(#8594,#8595,#8596,#8597,#8598,#8599,
#8600,#8601,#8602,#8603,#8604,#8605,#8606,#8607,#8608,#8609,#8610,#8611,
#8612,#8613,#8614,#8615),.UNSPECIFIED.,.F.,.F.,(4,2,2,2,2,2,2,2,2,2,4),
(0.671876099962389,0.714365153473771,0.756854206985153,0.841832314007917,
0.92482323197575,1.00781414994358,1.09080506791142,1.17379598587925,1.25877409290201,
1.3012631464134,1.34375219992478),.UNSPECIFIED.);
#431=B_SPLINE_CURVE_WITH_KNOTS('',3,(#8622,#8623,#8624,#8625,#8626,#8627,
#8628,#8629,#8630,#8631,#8632,#8633),.UNSPECIFIED.,.F.,.F.,(4,2,2,2,2,4),
(0.67187609996239,0.714365153473772,0.756854206985154,0.841832314007918,
0.924823231975752,1.00781414994359),.UNSPECIFIED.);
#432=B_SPLINE_CURVE_WITH_KNOTS('',3,(#8635,#8636,#8637,#8638,#8639,#8640,
#8641,#8642,#8643,#8644,#8645,#8646),.UNSPECIFIED.,.F.,.F.,(4,2,2,2,2,4),
(0.335938049981195,0.418928967949029,0.501919885916863,0.586897992939627,
0.629387046451009,0.67187609996239),.UNSPECIFIED.);
#433=B_SPLINE_CURVE_WITH_KNOTS('',3,(#8651,#8652,#8653,#8654,#8655,#8656,
#8657,#8658,#8659,#8660,#8661,#8662),.UNSPECIFIED.,.F.,.F.,(4,2,2,2,2,4),
(0.,0.042489053511382,0.0849781070227639,0.169956214045528,0.252947132013362,
0.335938049981195),.UNSPECIFIED.);
#434=B_SPLINE_CURVE_WITH_KNOTS('',3,(#8663,#8664,#8665,#8666,#8667,#8668,
#8669,#8670,#8671,#8672,#8673,#8674),.UNSPECIFIED.,.F.,.F.,(4,2,2,2,2,4),
(1.00781414994359,1.09080506791142,1.17379598587925,1.25877409290202,1.3012631464134,
1.34375219992478),.UNSPECIFIED.);
#435=B_SPLINE_CURVE_WITH_KNOTS('',3,(#8677,#8678,#8679,#8680,#8681,#8682,
#8683,#8684,#8685,#8686,#8687,#8688,#8689,#8690,#8691,#8692,#8693,#8694,
#8695,#8696,#8697,#8698),.UNSPECIFIED.,.F.,.F.,(4,2,2,2,2,2,2,2,2,2,4),
(0.,0.042489053511382,0.084978107022764,0.169956214045528,0.252947132013362,
0.335938049981195,0.418928967949029,0.501919885916863,0.586897992939627,
0.629387046451009,0.671876099962391),.UNSPECIFIED.);
#436=B_SPLINE_CURVE_WITH_KNOTS('',3,(#8699,#8700,#8701,#8702,#8703,#8704,
#8705,#8706,#8707,#8708,#8709,#8710,#8711,#8712,#8713,#8714,#8715,#8716,
#8717,#8718,#8719,#8720),.UNSPECIFIED.,.F.,.F.,(4,2,2,2,2,2,2,2,2,2,4),
(0.671876099962391,0.714365153473772,0.756854206985154,0.841832314007918,
0.924823231975752,1.00781414994359,1.09080506791142,1.17379598587925,1.25877409290202,
1.3012631464134,1.34375219992478),.UNSPECIFIED.);
#437=B_SPLINE_CURVE_WITH_KNOTS('',3,(#8726,#8727,#8728,#8729,#8730,#8731,
#8732,#8733,#8734,#8735,#8736,#8737,#8738,#8739,#8740,#8741,#8742,#8743,
#8744,#8745,#8746,#8747,#8748,#8749,#8750,#8751,#8752,#8753,#8754,#8755,
#8756,#8757),.UNSPECIFIED.,.F.,.F.,(4,2,2,2,2,2,2,2,2,2,2,2,2,2,2,4),(0.,
0.0424890535113821,0.0849781070227642,0.169956214045528,0.252947132013362,
0.335938049981195,0.418928967949028,0.501919885916861,0.586897992939625,
0.629387046451007,0.67187609996239,0.714365153473772,0.756854206985154,
0.841832314007918,0.924823231975751,1.00781414994358),.UNSPECIFIED.);
#438=B_SPLINE_CURVE_WITH_KNOTS('',3,(#8759,#8760,#8761,#8762,#8763,#8764,
#8765,#8766,#8767,#8768,#8769,#8770),.UNSPECIFIED.,.F.,.F.,(4,2,2,2,2,4),
(1.00781414994358,1.09080506791142,1.17379598587925,1.25877409290201,1.3012631464134,
1.34375219992478),.UNSPECIFIED.);
#439=B_SPLINE_CURVE_WITH_KNOTS('',3,(#8777,#8778,#8779,#8780,#8781,#8782,
#8783,#8784,#8785,#8786,#8787,#8788,#8789,#8790,#8791,#8792,#8793,#8794,
#8795,#8796,#8797,#8798),.UNSPECIFIED.,.F.,.F.,(4,2,2,2,2,2,2,2,2,2,4),
(0.335938049981195,0.418928967949028,0.501919885916861,0.586897992939625,
0.629387046451007,0.671876099962389,0.714365153473771,0.756854206985153,
0.841832314007918,0.924823231975751,1.00781414994358),.UNSPECIFIED.);
#440=B_SPLINE_CURVE_WITH_KNOTS('',3,(#8803,#8804,#8805,#8806,#8807,#8808,
#8809,#8810,#8811,#8812,#8813,#8814),.UNSPECIFIED.,.F.,.F.,(4,2,2,2,2,4),
(0.,0.0424890535113821,0.0849781070227642,0.169956214045528,0.252947132013361,
0.335938049981195),.UNSPECIFIED.);
#441=B_SPLINE_CURVE_WITH_KNOTS('',3,(#8815,#8816,#8817,#8818,#8819,#8820,
#8821,#8822,#8823,#8824,#8825,#8826),.UNSPECIFIED.,.F.,.F.,(4,2,2,2,2,4),
(1.00781414994358,1.09080506791142,1.17379598587925,1.25877409290201,1.3012631464134,
1.34375219992478),.UNSPECIFIED.);
#442=B_SPLINE_CURVE_WITH_KNOTS('',3,(#8833,#8834,#8835,#8836,#8837,#8838,
#8839,#8840,#8841,#8842,#8843,#8844,#8845,#8846,#8847,#8848,#8849,#8850,
#8851,#8852,#8853,#8854),.UNSPECIFIED.,.F.,.F.,(4,2,2,2,2,2,2,2,2,2,4),
(0.335938049981195,0.418928967949029,0.501919885916863,0.586897992939627,
0.629387046451009,0.67187609996239,0.714365153473772,0.756854206985154,
0.841832314007918,0.924823231975752,1.00781414994359),.UNSPECIFIED.);
#443=B_SPLINE_CURVE_WITH_KNOTS('',3,(#8859,#8860,#8861,#8862,#8863,#8864,
#8865,#8866,#8867,#8868,#8869,#8870),.UNSPECIFIED.,.F.,.F.,(4,2,2,2,2,4),
(0.,0.042489053511382,0.0849781070227639,0.169956214045528,0.252947132013361,
0.335938049981195),.UNSPECIFIED.);
#444=B_SPLINE_CURVE_WITH_KNOTS('',3,(#8871,#8872,#8873,#8874,#8875,#8876,
#8877,#8878,#8879,#8880,#8881,#8882),.UNSPECIFIED.,.F.,.F.,(4,2,2,2,2,4),
(1.00781414994359,1.09080506791142,1.17379598587925,1.25877409290202,1.3012631464134,
1.34375219992478),.UNSPECIFIED.);
#445=B_SPLINE_CURVE_WITH_KNOTS('',3,(#8885,#8886,#8887,#8888,#8889,#8890,
#8891,#8892,#8893,#8894,#8895,#8896,#8897,#8898,#8899,#8900,#8901,#8902,
#8903,#8904,#8905,#8906,#8907,#8908,#8909,#8910,#8911,#8912,#8913,#8914,
#8915,#8916),.UNSPECIFIED.,.F.,.F.,(4,2,2,2,2,2,2,2,2,2,2,2,2,2,2,4),(0.,
0.042489053511382,0.084978107022764,0.169956214045528,0.252947132013362,
0.335938049981195,0.418928967949029,0.501919885916863,0.586897992939627,
0.629387046451009,0.671876099962391,0.714365153473772,0.756854206985154,
0.841832314007918,0.924823231975752,1.00781414994359),.UNSPECIFIED.);
#446=B_SPLINE_CURVE_WITH_KNOTS('',3,(#8917,#8918,#8919,#8920,#8921,#8922,
#8923,#8924,#8925,#8926,#8927,#8928),.UNSPECIFIED.,.F.,.F.,(4,2,2,2,2,4),
(1.00781414994359,1.09080506791142,1.17379598587925,1.25877409290202,1.3012631464134,
1.34375219992478),.UNSPECIFIED.);
#447=SHAPE_REPRESENTATION_RELATIONSHIP('SRR','None',#10168,#469);
#448=SHAPE_REPRESENTATION_RELATIONSHIP('SRR','None',#10169,#470);
#449=SHAPE_REPRESENTATION_RELATIONSHIP('SRR','None',#10170,#471);
#450=SHAPE_REPRESENTATION_RELATIONSHIP('SRR','None',#10171,#472);
#451=SHAPE_REPRESENTATION_RELATIONSHIP('SRR','None',#10172,#473);
#452=SHAPE_REPRESENTATION_RELATIONSHIP('SRR','None',#10173,#474);
#453=SHAPE_REPRESENTATION_RELATIONSHIP('SRR','None',#10174,#475);
#454=SHAPE_REPRESENTATION_RELATIONSHIP('SRR','None',#10175,#476);
#455=SHAPE_REPRESENTATION_RELATIONSHIP('SRR','None',#10176,#477);
#456=SHAPE_REPRESENTATION_RELATIONSHIP('SRR','None',#10177,#478);
#457=SHAPE_REPRESENTATION_RELATIONSHIP('SRR','None',#10178,#479);
#458=SHAPE_REPRESENTATION_RELATIONSHIP('SRR','None',#10179,#480);
#459=SHAPE_REPRESENTATION_RELATIONSHIP('SRR','None',#10180,#481);
#460=SHAPE_REPRESENTATION_RELATIONSHIP('SRR','None',#10181,#482);
#461=SHAPE_REPRESENTATION_RELATIONSHIP('SRR','None',#10182,#483);
#462=SHAPE_REPRESENTATION_RELATIONSHIP('SRR','None',#10183,#484);
#463=SHAPE_REPRESENTATION_RELATIONSHIP('SRR','None',#10184,#485);
#464=SHAPE_REPRESENTATION_RELATIONSHIP('SRR','None',#10185,#486);
#465=SHAPE_REPRESENTATION_RELATIONSHIP('SRR','None',#10186,#487);
#466=SHAPE_REPRESENTATION_RELATIONSHIP('SRR','None',#10187,#488);
#467=SHAPE_REPRESENTATION_RELATIONSHIP('SRR','None',#10188,#489);
#468=SHAPE_REPRESENTATION_RELATIONSHIP('SRR','None',#10189,#490);
#469=ADVANCED_BREP_SHAPE_REPRESENTATION('',(#513),#9997);
#470=ADVANCED_BREP_SHAPE_REPRESENTATION('',(#514),#9998);
#471=ADVANCED_BREP_SHAPE_REPRESENTATION('',(#515),#9999);
#472=ADVANCED_BREP_SHAPE_REPRESENTATION('',(#516),#10000);
#473=ADVANCED_BREP_SHAPE_REPRESENTATION('',(#517),#10001);
#474=ADVANCED_BREP_SHAPE_REPRESENTATION('',(#518),#10002);
#475=ADVANCED_BREP_SHAPE_REPRESENTATION('',(#519),#10003);
#476=ADVANCED_BREP_SHAPE_REPRESENTATION('',(#520),#10004);
#477=ADVANCED_BREP_SHAPE_REPRESENTATION('',(#521),#10005);
#478=ADVANCED_BREP_SHAPE_REPRESENTATION('',(#522),#10006);
#479=ADVANCED_BREP_SHAPE_REPRESENTATION('',(#523),#10007);
#480=ADVANCED_BREP_SHAPE_REPRESENTATION('',(#524),#10008);
#481=ADVANCED_BREP_SHAPE_REPRESENTATION('',(#525),#10009);
#482=ADVANCED_BREP_SHAPE_REPRESENTATION('',(#526),#10010);
#483=ADVANCED_BREP_SHAPE_REPRESENTATION('',(#527),#10011);
#484=ADVANCED_BREP_SHAPE_REPRESENTATION('',(#421),#10012);
#485=ADVANCED_BREP_SHAPE_REPRESENTATION('',(#422),#10013);
#486=ADVANCED_BREP_SHAPE_REPRESENTATION('',(#528),#10014);
#487=ADVANCED_BREP_SHAPE_REPRESENTATION('',(#529),#10015);
#488=ADVANCED_BREP_SHAPE_REPRESENTATION('',(#423),#10016);
#489=ADVANCED_BREP_SHAPE_REPRESENTATION('',(#530),#10017);
#490=ADVANCED_BREP_SHAPE_REPRESENTATION('',(#424),#10018);
#491=STYLED_ITEM('',(#10362),#513);
#492=STYLED_ITEM('',(#10341),#514);
#493=STYLED_ITEM('',(#10362),#515);
#494=STYLED_ITEM('',(#10341),#516);
#495=STYLED_ITEM('',(#10362),#517);
#496=STYLED_ITEM('',(#10341),#518);
#497=STYLED_ITEM('',(#10362),#519);
#498=STYLED_ITEM('',(#10341),#520);
#499=STYLED_ITEM('',(#10341),#521);
#500=STYLED_ITEM('',(#10341),#522);
#501=STYLED_ITEM('',(#10327),#523);
#502=STYLED_ITEM('',(#10327),#524);
#503=STYLED_ITEM('',(#10334),#525);
#504=STYLED_ITEM('',(#10334),#526);
#505=STYLED_ITEM('',(#10362),#527);
#506=STYLED_ITEM('',(#10355),#421);
#507=STYLED_ITEM('',(#10355),#422);
#508=STYLED_ITEM('',(#10355),#528);
#509=STYLED_ITEM('',(#10355),#529);
#510=STYLED_ITEM('',(#10355),#423);
#511=STYLED_ITEM('',(#10355),#530);
#512=STYLED_ITEM('',(#10355),#424);
#513=MANIFOLD_SOLID_BREP('Body1',#5613);
#514=MANIFOLD_SOLID_BREP('Body1',#5614);
#515=MANIFOLD_SOLID_BREP('Body1',#5615);
#516=MANIFOLD_SOLID_BREP('Body1',#5616);
#517=MANIFOLD_SOLID_BREP('Body1',#5617);
#518=MANIFOLD_SOLID_BREP('Body1',#5618);
#519=MANIFOLD_SOLID_BREP('Body1',#5619);
#520=MANIFOLD_SOLID_BREP('Body1',#5620);
#521=MANIFOLD_SOLID_BREP('Body1',#5621);
#522=MANIFOLD_SOLID_BREP('Body1',#5622);
#523=MANIFOLD_SOLID_BREP('Body1',#5623);
#524=MANIFOLD_SOLID_BREP('Body1',#5624);
#525=MANIFOLD_SOLID_BREP('Body1',#5625);
#526=MANIFOLD_SOLID_BREP('Body1',#5626);
#527=MANIFOLD_SOLID_BREP('Body1',#5627);
#528=MANIFOLD_SOLID_BREP('Body1',#5632);
#529=MANIFOLD_SOLID_BREP('Body1',#5633);
#530=MANIFOLD_SOLID_BREP('Body1',#5636);
#531=FACE_BOUND('',#1120,.T.);
#532=FACE_BOUND('',#1122,.T.);
#533=FACE_BOUND('',#1126,.T.);
#534=FACE_BOUND('',#1128,.T.);
#535=FACE_BOUND('',#1132,.T.);
#536=FACE_BOUND('',#1134,.T.);
#537=FACE_BOUND('',#1138,.T.);
#538=FACE_BOUND('',#1140,.T.);
#539=FACE_BOUND('',#1144,.T.);
#540=FACE_BOUND('',#1146,.T.);
#541=FACE_BOUND('',#1150,.T.);
#542=FACE_BOUND('',#1152,.T.);
#543=FACE_BOUND('',#1156,.T.);
#544=FACE_BOUND('',#1158,.T.);
#545=FACE_BOUND('',#1162,.T.);
#546=FACE_BOUND('',#1164,.T.);
#547=FACE_BOUND('',#1167,.T.);
#548=FACE_BOUND('',#1170,.T.);
#549=FACE_BOUND('',#1173,.T.);
#550=FACE_BOUND('',#1176,.T.);
#551=FACE_BOUND('',#1186,.T.);
#552=FACE_BOUND('',#1187,.T.);
#553=FACE_BOUND('',#1188,.T.);
#554=FACE_BOUND('',#1189,.T.);
#555=FACE_BOUND('',#1191,.T.);
#556=FACE_BOUND('',#1192,.T.);
#557=FACE_BOUND('',#1193,.T.);
#558=FACE_BOUND('',#1194,.T.);
#559=FACE_BOUND('',#1203,.T.);
#560=FACE_BOUND('',#1204,.T.);
#561=FACE_BOUND('',#1205,.T.);
#562=FACE_BOUND('',#1206,.T.);
#563=FACE_BOUND('',#1217,.T.);
#564=FACE_BOUND('',#1218,.T.);
#565=FACE_BOUND('',#1219,.T.);
#566=FACE_BOUND('',#1220,.T.);
#567=FACE_BOUND('',#1225,.T.);
#568=FACE_BOUND('',#1228,.T.);
#569=FACE_BOUND('',#1230,.T.);
#570=FACE_BOUND('',#1231,.T.);
#571=FACE_BOUND('',#1234,.T.);
#572=FACE_BOUND('',#1235,.T.);
#573=FACE_BOUND('',#1242,.T.);
#574=FACE_BOUND('',#1245,.T.);
#575=FACE_BOUND('',#1247,.T.);
#576=FACE_BOUND('',#1248,.T.);
#577=FACE_BOUND('',#1251,.T.);
#578=FACE_BOUND('',#1252,.T.);
#579=FACE_BOUND('',#1262,.T.);
#580=FACE_BOUND('',#1263,.T.);
#581=FACE_BOUND('',#1265,.T.);
#582=FACE_BOUND('',#1266,.T.);
#583=FACE_BOUND('',#1268,.T.);
#584=FACE_BOUND('',#1270,.T.);
#585=FACE_BOUND('',#1274,.T.);
#586=FACE_BOUND('',#1276,.T.);
#587=FACE_BOUND('',#1284,.T.);
#588=FACE_BOUND('',#1285,.T.);
#589=FACE_BOUND('',#1295,.T.);
#590=FACE_BOUND('',#1296,.T.);
#591=FACE_BOUND('',#1306,.T.);
#592=FACE_BOUND('',#1307,.T.);
#593=FACE_BOUND('',#1317,.T.);
#594=FACE_BOUND('',#1318,.T.);
#595=FACE_BOUND('',#1333,.T.);
#596=FACE_BOUND('',#1335,.T.);
#597=FACE_BOUND('',#1337,.T.);
#598=FACE_BOUND('',#1384,.T.);
#599=FACE_BOUND('',#1394,.T.);
#600=FACE_BOUND('',#1402,.T.);
#601=FACE_BOUND('',#1410,.T.);
#602=FACE_BOUND('',#1426,.T.);
#603=FACE_BOUND('',#1441,.T.);
#604=FACE_BOUND('',#1444,.T.);
#605=FACE_BOUND('',#1459,.T.);
#606=FACE_BOUND('',#1465,.T.);
#607=FACE_BOUND('',#1468,.T.);
#608=FACE_BOUND('',#1474,.T.);
#609=PLANE('',#5890);
#610=PLANE('',#5891);
#611=PLANE('',#5899);
#612=PLANE('',#5900);
#613=PLANE('',#5908);
#614=PLANE('',#5909);
#615=PLANE('',#5917);
#616=PLANE('',#5918);
#617=PLANE('',#5926);
#618=PLANE('',#5927);
#619=PLANE('',#5935);
#620=PLANE('',#5936);
#621=PLANE('',#5944);
#622=PLANE('',#5945);
#623=PLANE('',#5953);
#624=PLANE('',#5954);
#625=PLANE('',#5959);
#626=PLANE('',#5964);
#627=PLANE('',#5969);
#628=PLANE('',#5974);
#629=PLANE('',#5984);
#630=PLANE('',#5985);
#631=PLANE('',#5986);
#632=PLANE('',#5987);
#633=PLANE('',#5988);
#634=PLANE('',#5989);
#635=PLANE('',#6003);
#636=PLANE('',#6004);
#637=PLANE('',#6005);
#638=PLANE('',#6006);
#639=PLANE('',#6007);
#640=PLANE('',#6008);
#641=PLANE('',#6009);
#642=PLANE('',#6010);
#643=PLANE('',#6011);
#644=PLANE('',#6012);
#645=PLANE('',#6013);
#646=PLANE('',#6014);
#647=PLANE('',#6015);
#648=PLANE('',#6016);
#649=PLANE('',#6027);
#650=PLANE('',#6028);
#651=PLANE('',#6029);
#652=PLANE('',#6030);
#653=PLANE('',#6031);
#654=PLANE('',#6032);
#655=PLANE('',#6033);
#656=PLANE('',#6034);
#657=PLANE('',#6045);
#658=PLANE('',#6046);
#659=PLANE('',#6047);
#660=PLANE('',#6048);
#661=PLANE('',#6049);
#662=PLANE('',#6050);
#663=PLANE('',#6051);
#664=PLANE('',#6052);
#665=PLANE('',#6060);
#666=PLANE('',#6061);
#667=PLANE('',#6062);
#668=PLANE('',#6063);
#669=PLANE('',#6064);
#670=PLANE('',#6065);
#671=PLANE('',#6084);
#672=PLANE('',#6085);
#673=PLANE('',#6086);
#674=PLANE('',#6087);
#675=PLANE('',#6088);
#676=PLANE('',#6089);
#677=PLANE('',#6090);
#678=PLANE('',#6091);
#679=PLANE('',#6092);
#680=PLANE('',#6093);
#681=PLANE('',#6094);
#682=PLANE('',#6095);
#683=PLANE('',#6096);
#684=PLANE('',#6097);
#685=PLANE('',#6098);
#686=PLANE('',#6099);
#687=PLANE('',#6100);
#688=PLANE('',#6101);
#689=PLANE('',#6102);
#690=PLANE('',#6103);
#691=PLANE('',#6104);
#692=PLANE('',#6105);
#693=PLANE('',#6106);
#694=PLANE('',#6107);
#695=PLANE('',#6108);
#696=PLANE('',#6109);
#697=PLANE('',#6110);
#698=PLANE('',#6111);
#699=PLANE('',#6112);
#700=PLANE('',#6113);
#701=PLANE('',#6114);
#702=PLANE('',#6115);
#703=PLANE('',#6116);
#704=PLANE('',#6117);
#705=PLANE('',#6118);
#706=PLANE('',#6119);
#707=PLANE('',#6122);
#708=PLANE('',#6123);
#709=PLANE('',#6124);
#710=PLANE('',#6125);
#711=PLANE('',#6126);
#712=PLANE('',#6127);
#713=PLANE('',#6128);
#714=PLANE('',#6129);
#715=PLANE('',#6130);
#716=PLANE('',#6131);
#717=PLANE('',#6133);
#718=PLANE('',#6135);
#719=PLANE('',#6136);
#720=PLANE('',#6137);
#721=PLANE('',#6138);
#722=PLANE('',#6139);
#723=PLANE('',#6140);
#724=PLANE('',#6141);
#725=PLANE('',#6142);
#726=PLANE('',#6143);
#727=PLANE('',#6144);
#728=PLANE('',#6145);
#729=PLANE('',#6146);
#730=PLANE('',#6147);
#731=PLANE('',#6148);
#732=PLANE('',#6149);
#733=PLANE('',#6150);
#734=PLANE('',#6151);
#735=PLANE('',#6152);
#736=PLANE('',#6153);
#737=PLANE('',#6154);
#738=PLANE('',#6155);
#739=PLANE('',#6156);
#740=PLANE('',#6157);
#741=PLANE('',#6158);
#742=PLANE('',#6159);
#743=PLANE('',#6160);
#744=PLANE('',#6161);
#745=PLANE('',#6162);
#746=PLANE('',#6163);
#747=PLANE('',#6164);
#748=PLANE('',#6165);
#749=PLANE('',#6166);
#750=PLANE('',#6167);
#751=PLANE('',#6168);
#752=PLANE('',#6169);
#753=PLANE('',#6170);
#754=PLANE('',#6171);
#755=PLANE('',#6172);
#756=PLANE('',#6173);
#757=PLANE('',#6174);
#758=PLANE('',#6177);
#759=PLANE('',#6178);
#760=PLANE('',#6179);
#761=PLANE('',#6180);
#762=PLANE('',#6181);
#763=PLANE('',#6183);
#764=PLANE('',#6184);
#765=PLANE('',#6185);
#766=PLANE('',#6186);
#767=PLANE('',#6187);
#768=PLANE('',#6188);
#769=PLANE('',#6189);
#770=PLANE('',#6190);
#771=PLANE('',#6191);
#772=PLANE('',#6196);
#773=PLANE('',#6197);
#774=PLANE('',#6205);
#775=PLANE('',#6211);
#776=PLANE('',#6219);
#777=PLANE('',#6227);
#778=PLANE('',#6228);
#779=PLANE('',#6229);
#780=PLANE('',#6230);
#781=PLANE('',#6231);
#782=PLANE('',#6232);
#783=PLANE('',#6233);
#784=PLANE('',#6234);
#785=PLANE('',#6235);
#786=PLANE('',#6237);
#787=PLANE('',#6238);
#788=PLANE('',#6239);
#789=PLANE('',#6241);
#790=PLANE('',#6242);
#791=PLANE('',#6243);
#792=PLANE('',#6244);
#793=PLANE('',#6245);
#794=PLANE('',#6246);
#795=PLANE('',#6253);
#796=PLANE('',#6254);
#797=PLANE('',#6255);
#798=PLANE('',#6256);
#799=PLANE('',#6263);
#800=PLANE('',#6267);
#801=PLANE('',#6269);
#802=PLANE('',#6270);
#803=PLANE('',#6271);
#804=PLANE('',#6272);
#805=PLANE('',#6273);
#806=PLANE('',#6274);
#807=PLANE('',#6275);
#808=PLANE('',#6276);
#809=PLANE('',#6277);
#810=PLANE('',#6279);
#811=PLANE('',#6287);
#812=PLANE('',#6298);
#813=PLANE('',#6302);
#814=PLANE('',#6304);
#815=PLANE('',#6312);
#816=PLANE('',#6320);
#817=PLANE('',#6321);
#818=PLANE('',#6322);
#819=PLANE('',#6323);
#820=PLANE('',#6324);
#821=PLANE('',#6325);
#822=PLANE('',#6326);
#823=PLANE('',#6327);
#824=PLANE('',#6328);
#825=FACE_OUTER_BOUND('',#1117,.T.);
#826=FACE_OUTER_BOUND('',#1118,.T.);
#827=FACE_OUTER_BOUND('',#1119,.T.);
#828=FACE_OUTER_BOUND('',#1121,.T.);
#829=FACE_OUTER_BOUND('',#1123,.T.);
#830=FACE_OUTER_BOUND('',#1124,.T.);
#831=FACE_OUTER_BOUND('',#1125,.T.);
#832=FACE_OUTER_BOUND('',#1127,.T.);
#833=FACE_OUTER_BOUND('',#1129,.T.);
#834=FACE_OUTER_BOUND('',#1130,.T.);
#835=FACE_OUTER_BOUND('',#1131,.T.);
#836=FACE_OUTER_BOUND('',#1133,.T.);
#837=FACE_OUTER_BOUND('',#1135,.T.);
#838=FACE_OUTER_BOUND('',#1136,.T.);
#839=FACE_OUTER_BOUND('',#1137,.T.);
#840=FACE_OUTER_BOUND('',#1139,.T.);
#841=FACE_OUTER_BOUND('',#1141,.T.);
#842=FACE_OUTER_BOUND('',#1142,.T.);
#843=FACE_OUTER_BOUND('',#1143,.T.);
#844=FACE_OUTER_BOUND('',#1145,.T.);
#845=FACE_OUTER_BOUND('',#1147,.T.);
#846=FACE_OUTER_BOUND('',#1148,.T.);
#847=FACE_OUTER_BOUND('',#1149,.T.);
#848=FACE_OUTER_BOUND('',#1151,.T.);
#849=FACE_OUTER_BOUND('',#1153,.T.);
#850=FACE_OUTER_BOUND('',#1154,.T.);
#851=FACE_OUTER_BOUND('',#1155,.T.);
#852=FACE_OUTER_BOUND('',#1157,.T.);
#853=FACE_OUTER_BOUND('',#1159,.T.);
#854=FACE_OUTER_BOUND('',#1160,.T.);
#855=FACE_OUTER_BOUND('',#1161,.T.);
#856=FACE_OUTER_BOUND('',#1163,.T.);
#857=FACE_OUTER_BOUND('',#1165,.T.);
#858=FACE_OUTER_BOUND('',#1166,.T.);
#859=FACE_OUTER_BOUND('',#1168,.T.);
#860=FACE_OUTER_BOUND('',#1169,.T.);
#861=FACE_OUTER_BOUND('',#1171,.T.);
#862=FACE_OUTER_BOUND('',#1172,.T.);
#863=FACE_OUTER_BOUND('',#1174,.T.);
#864=FACE_OUTER_BOUND('',#1175,.T.);
#865=FACE_OUTER_BOUND('',#1177,.T.);
#866=FACE_OUTER_BOUND('',#1178,.T.);
#867=FACE_OUTER_BOUND('',#1179,.T.);
#868=FACE_OUTER_BOUND('',#1180,.T.);
#869=FACE_OUTER_BOUND('',#1181,.T.);
#870=FACE_OUTER_BOUND('',#1182,.T.);
#871=FACE_OUTER_BOUND('',#1183,.T.);
#872=FACE_OUTER_BOUND('',#1184,.T.);
#873=FACE_OUTER_BOUND('',#1185,.T.);
#874=FACE_OUTER_BOUND('',#1190,.T.);
#875=FACE_OUTER_BOUND('',#1195,.T.);
#876=FACE_OUTER_BOUND('',#1196,.T.);
#877=FACE_OUTER_BOUND('',#1197,.T.);
#878=FACE_OUTER_BOUND('',#1198,.T.);
#879=FACE_OUTER_BOUND('',#1199,.T.);
#880=FACE_OUTER_BOUND('',#1200,.T.);
#881=FACE_OUTER_BOUND('',#1201,.T.);
#882=FACE_OUTER_BOUND('',#1202,.T.);
#883=FACE_OUTER_BOUND('',#1207,.T.);
#884=FACE_OUTER_BOUND('',#1208,.T.);
#885=FACE_OUTER_BOUND('',#1209,.T.);
#886=FACE_OUTER_BOUND('',#1210,.T.);
#887=FACE_OUTER_BOUND('',#1211,.T.);
#888=FACE_OUTER_BOUND('',#1212,.T.);
#889=FACE_OUTER_BOUND('',#1213,.T.);
#890=FACE_OUTER_BOUND('',#1214,.T.);
#891=FACE_OUTER_BOUND('',#1215,.T.);
#892=FACE_OUTER_BOUND('',#1216,.T.);
#893=FACE_OUTER_BOUND('',#1221,.T.);
#894=FACE_OUTER_BOUND('',#1222,.T.);
#895=FACE_OUTER_BOUND('',#1223,.T.);
#896=FACE_OUTER_BOUND('',#1224,.T.);
#897=FACE_OUTER_BOUND('',#1226,.T.);
#898=FACE_OUTER_BOUND('',#1227,.T.);
#899=FACE_OUTER_BOUND('',#1229,.T.);
#900=FACE_OUTER_BOUND('',#1232,.T.);
#901=FACE_OUTER_BOUND('',#1233,.T.);
#902=FACE_OUTER_BOUND('',#1236,.T.);
#903=FACE_OUTER_BOUND('',#1237,.T.);
#904=FACE_OUTER_BOUND('',#1238,.T.);
#905=FACE_OUTER_BOUND('',#1239,.T.);
#906=FACE_OUTER_BOUND('',#1240,.T.);
#907=FACE_OUTER_BOUND('',#1241,.T.);
#908=FACE_OUTER_BOUND('',#1243,.T.);
#909=FACE_OUTER_BOUND('',#1244,.T.);
#910=FACE_OUTER_BOUND('',#1246,.T.);
#911=FACE_OUTER_BOUND('',#1249,.T.);
#912=FACE_OUTER_BOUND('',#1250,.T.);
#913=FACE_OUTER_BOUND('',#1253,.T.);
#914=FACE_OUTER_BOUND('',#1254,.T.);
#915=FACE_OUTER_BOUND('',#1255,.T.);
#916=FACE_OUTER_BOUND('',#1256,.T.);
#917=FACE_OUTER_BOUND('',#1257,.T.);
#918=FACE_OUTER_BOUND('',#1258,.T.);
#919=FACE_OUTER_BOUND('',#1259,.T.);
#920=FACE_OUTER_BOUND('',#1260,.T.);
#921=FACE_OUTER_BOUND('',#1261,.T.);
#922=FACE_OUTER_BOUND('',#1264,.T.);
#923=FACE_OUTER_BOUND('',#1267,.T.);
#924=FACE_OUTER_BOUND('',#1269,.T.);
#925=FACE_OUTER_BOUND('',#1271,.T.);
#926=FACE_OUTER_BOUND('',#1272,.T.);
#927=FACE_OUTER_BOUND('',#1273,.T.);
#928=FACE_OUTER_BOUND('',#1275,.T.);
#929=FACE_OUTER_BOUND('',#1277,.T.);
#930=FACE_OUTER_BOUND('',#1278,.T.);
#931=FACE_OUTER_BOUND('',#1279,.T.);
#932=FACE_OUTER_BOUND('',#1280,.T.);
#933=FACE_OUTER_BOUND('',#1281,.T.);
#934=FACE_OUTER_BOUND('',#1282,.T.);
#935=FACE_OUTER_BOUND('',#1283,.T.);
#936=FACE_OUTER_BOUND('',#1286,.T.);
#937=FACE_OUTER_BOUND('',#1287,.T.);
#938=FACE_OUTER_BOUND('',#1288,.T.);
#939=FACE_OUTER_BOUND('',#1289,.T.);
#940=FACE_OUTER_BOUND('',#1290,.T.);
#941=FACE_OUTER_BOUND('',#1291,.T.);
#942=FACE_OUTER_BOUND('',#1292,.T.);
#943=FACE_OUTER_BOUND('',#1293,.T.);
#944=FACE_OUTER_BOUND('',#1294,.T.);
#945=FACE_OUTER_BOUND('',#1297,.T.);
#946=FACE_OUTER_BOUND('',#1298,.T.);
#947=FACE_OUTER_BOUND('',#1299,.T.);
#948=FACE_OUTER_BOUND('',#1300,.T.);
#949=FACE_OUTER_BOUND('',#1301,.T.);
#950=FACE_OUTER_BOUND('',#1302,.T.);
#951=FACE_OUTER_BOUND('',#1303,.T.);
#952=FACE_OUTER_BOUND('',#1304,.T.);
#953=FACE_OUTER_BOUND('',#1305,.T.);
#954=FACE_OUTER_BOUND('',#1308,.T.);
#955=FACE_OUTER_BOUND('',#1309,.T.);
#956=FACE_OUTER_BOUND('',#1310,.T.);
#957=FACE_OUTER_BOUND('',#1311,.T.);
#958=FACE_OUTER_BOUND('',#1312,.T.);
#959=FACE_OUTER_BOUND('',#1313,.T.);
#960=FACE_OUTER_BOUND('',#1314,.T.);
#961=FACE_OUTER_BOUND('',#1315,.T.);
#962=FACE_OUTER_BOUND('',#1316,.T.);
#963=FACE_OUTER_BOUND('',#1319,.T.);
#964=FACE_OUTER_BOUND('',#1320,.T.);
#965=FACE_OUTER_BOUND('',#1321,.T.);
#966=FACE_OUTER_BOUND('',#1322,.T.);
#967=FACE_OUTER_BOUND('',#1323,.T.);
#968=FACE_OUTER_BOUND('',#1324,.T.);
#969=FACE_OUTER_BOUND('',#1325,.T.);
#970=FACE_OUTER_BOUND('',#1326,.T.);
#971=FACE_OUTER_BOUND('',#1327,.T.);
#972=FACE_OUTER_BOUND('',#1328,.T.);
#973=FACE_OUTER_BOUND('',#1329,.T.);
#974=FACE_OUTER_BOUND('',#1330,.T.);
#975=FACE_OUTER_BOUND('',#1331,.T.);
#976=FACE_OUTER_BOUND('',#1332,.T.);
#977=FACE_OUTER_BOUND('',#1334,.T.);
#978=FACE_OUTER_BOUND('',#1336,.T.);
#979=FACE_OUTER_BOUND('',#1338,.T.);
#980=FACE_OUTER_BOUND('',#1339,.T.);
#981=FACE_OUTER_BOUND('',#1340,.T.);
#982=FACE_OUTER_BOUND('',#1341,.T.);
#983=FACE_OUTER_BOUND('',#1342,.T.);
#984=FACE_OUTER_BOUND('',#1343,.T.);
#985=FACE_OUTER_BOUND('',#1344,.T.);
#986=FACE_OUTER_BOUND('',#1345,.T.);
#987=FACE_OUTER_BOUND('',#1346,.T.);
#988=FACE_OUTER_BOUND('',#1347,.T.);
#989=FACE_OUTER_BOUND('',#1348,.T.);
#990=FACE_OUTER_BOUND('',#1349,.T.);
#991=FACE_OUTER_BOUND('',#1350,.T.);
#992=FACE_OUTER_BOUND('',#1351,.T.);
#993=FACE_OUTER_BOUND('',#1352,.T.);
#994=FACE_OUTER_BOUND('',#1353,.T.);
#995=FACE_OUTER_BOUND('',#1354,.T.);
#996=FACE_OUTER_BOUND('',#1355,.T.);
#997=FACE_OUTER_BOUND('',#1356,.T.);
#998=FACE_OUTER_BOUND('',#1357,.T.);
#999=FACE_OUTER_BOUND('',#1358,.T.);
#1000=FACE_OUTER_BOUND('',#1359,.T.);
#1001=FACE_OUTER_BOUND('',#1360,.T.);
#1002=FACE_OUTER_BOUND('',#1361,.T.);
#1003=FACE_OUTER_BOUND('',#1362,.T.);
#1004=FACE_OUTER_BOUND('',#1363,.T.);
#1005=FACE_OUTER_BOUND('',#1364,.T.);
#1006=FACE_OUTER_BOUND('',#1365,.T.);
#1007=FACE_OUTER_BOUND('',#1366,.T.);
#1008=FACE_OUTER_BOUND('',#1367,.T.);
#1009=FACE_OUTER_BOUND('',#1368,.T.);
#1010=FACE_OUTER_BOUND('',#1369,.T.);
#1011=FACE_OUTER_BOUND('',#1370,.T.);
#1012=FACE_OUTER_BOUND('',#1371,.T.);
#1013=FACE_OUTER_BOUND('',#1372,.T.);
#1014=FACE_OUTER_BOUND('',#1373,.T.);
#1015=FACE_OUTER_BOUND('',#1374,.T.);
#1016=FACE_OUTER_BOUND('',#1375,.T.);
#1017=FACE_OUTER_BOUND('',#1376,.T.);
#1018=FACE_OUTER_BOUND('',#1377,.T.);
#1019=FACE_OUTER_BOUND('',#1378,.T.);
#1020=FACE_OUTER_BOUND('',#1379,.T.);
#1021=FACE_OUTER_BOUND('',#1380,.T.);
#1022=FACE_OUTER_BOUND('',#1381,.T.);
#1023=FACE_OUTER_BOUND('',#1382,.T.);
#1024=FACE_OUTER_BOUND('',#1383,.T.);
#1025=FACE_OUTER_BOUND('',#1385,.T.);
#1026=FACE_OUTER_BOUND('',#1386,.T.);
#1027=FACE_OUTER_BOUND('',#1387,.T.);
#1028=FACE_OUTER_BOUND('',#1388,.T.);
#1029=FACE_OUTER_BOUND('',#1389,.T.);
#1030=FACE_OUTER_BOUND('',#1390,.T.);
#1031=FACE_OUTER_BOUND('',#1391,.T.);
#1032=FACE_OUTER_BOUND('',#1392,.T.);
#1033=FACE_OUTER_BOUND('',#1393,.T.);
#1034=FACE_OUTER_BOUND('',#1395,.T.);
#1035=FACE_OUTER_BOUND('',#1396,.T.);
#1036=FACE_OUTER_BOUND('',#1397,.T.);
#1037=FACE_OUTER_BOUND('',#1398,.T.);
#1038=FACE_OUTER_BOUND('',#1399,.T.);
#1039=FACE_OUTER_BOUND('',#1400,.T.);
#1040=FACE_OUTER_BOUND('',#1401,.T.);
#1041=FACE_OUTER_BOUND('',#1403,.T.);
#1042=FACE_OUTER_BOUND('',#1404,.T.);
#1043=FACE_OUTER_BOUND('',#1405,.T.);
#1044=FACE_OUTER_BOUND('',#1406,.T.);
#1045=FACE_OUTER_BOUND('',#1407,.T.);
#1046=FACE_OUTER_BOUND('',#1408,.T.);
#1047=FACE_OUTER_BOUND('',#1409,.T.);
#1048=FACE_OUTER_BOUND('',#1411,.T.);
#1049=FACE_OUTER_BOUND('',#1412,.T.);
#1050=FACE_OUTER_BOUND('',#1413,.T.);
#1051=FACE_OUTER_BOUND('',#1414,.T.);
#1052=FACE_OUTER_BOUND('',#1415,.T.);
#1053=FACE_OUTER_BOUND('',#1416,.T.);
#1054=FACE_OUTER_BOUND('',#1417,.T.);
#1055=FACE_OUTER_BOUND('',#1418,.T.);
#1056=FACE_OUTER_BOUND('',#1419,.T.);
#1057=FACE_OUTER_BOUND('',#1420,.T.);
#1058=FACE_OUTER_BOUND('',#1421,.T.);
#1059=FACE_OUTER_BOUND('',#1422,.T.);
#1060=FACE_OUTER_BOUND('',#1423,.T.);
#1061=FACE_OUTER_BOUND('',#1424,.T.);
#1062=FACE_OUTER_BOUND('',#1425,.T.);
#1063=FACE_OUTER_BOUND('',#1427,.T.);
#1064=FACE_OUTER_BOUND('',#1428,.T.);
#1065=FACE_OUTER_BOUND('',#1429,.T.);
#1066=FACE_OUTER_BOUND('',#1430,.T.);
#1067=FACE_OUTER_BOUND('',#1431,.T.);
#1068=FACE_OUTER_BOUND('',#1432,.T.);
#1069=FACE_OUTER_BOUND('',#1433,.T.);
#1070=FACE_OUTER_BOUND('',#1434,.T.);
#1071=FACE_OUTER_BOUND('',#1435,.T.);
#1072=FACE_OUTER_BOUND('',#1436,.T.);
#1073=FACE_OUTER_BOUND('',#1437,.T.);
#1074=FACE_OUTER_BOUND('',#1438,.T.);
#1075=FACE_OUTER_BOUND('',#1439,.T.);
#1076=FACE_OUTER_BOUND('',#1440,.T.);
#1077=FACE_OUTER_BOUND('',#1442,.T.);
#1078=FACE_OUTER_BOUND('',#1443,.T.);
#1079=FACE_OUTER_BOUND('',#1445,.T.);
#1080=FACE_OUTER_BOUND('',#1446,.T.);
#1081=FACE_OUTER_BOUND('',#1447,.T.);
#1082=FACE_OUTER_BOUND('',#1448,.T.);
#1083=FACE_OUTER_BOUND('',#1449,.T.);
#1084=FACE_OUTER_BOUND('',#1450,.T.);
#1085=FACE_OUTER_BOUND('',#1451,.T.);
#1086=FACE_OUTER_BOUND('',#1452,.T.);
#1087=FACE_OUTER_BOUND('',#1453,.T.);
#1088=FACE_OUTER_BOUND('',#1454,.T.);
#1089=FACE_OUTER_BOUND('',#1455,.T.);
#1090=FACE_OUTER_BOUND('',#1456,.T.);
#1091=FACE_OUTER_BOUND('',#1457,.T.);
#1092=FACE_OUTER_BOUND('',#1458,.T.);
#1093=FACE_OUTER_BOUND('',#1460,.T.);
#1094=FACE_OUTER_BOUND('',#1461,.T.);
#1095=FACE_OUTER_BOUND('',#1462,.T.);
#1096=FACE_OUTER_BOUND('',#1463,.T.);
#1097=FACE_OUTER_BOUND('',#1464,.T.);
#1098=FACE_OUTER_BOUND('',#1466,.T.);
#1099=FACE_OUTER_BOUND('',#1467,.T.);
#1100=FACE_OUTER_BOUND('',#1469,.T.);
#1101=FACE_OUTER_BOUND('',#1470,.T.);
#1102=FACE_OUTER_BOUND('',#1471,.T.);
#1103=FACE_OUTER_BOUND('',#1472,.T.);
#1104=FACE_OUTER_BOUND('',#1473,.T.);
#1105=FACE_OUTER_BOUND('',#1475,.T.);
#1106=FACE_OUTER_BOUND('',#1476,.T.);
#1107=FACE_OUTER_BOUND('',#1477,.T.);
#1108=FACE_OUTER_BOUND('',#1478,.T.);
#1109=FACE_OUTER_BOUND('',#1479,.T.);
#1110=FACE_OUTER_BOUND('',#1480,.T.);
#1111=FACE_OUTER_BOUND('',#1481,.T.);
#1112=FACE_OUTER_BOUND('',#1482,.T.);
#1113=FACE_OUTER_BOUND('',#1483,.T.);
#1114=FACE_OUTER_BOUND('',#1484,.T.);
#1115=FACE_OUTER_BOUND('',#1485,.T.);
#1116=FACE_OUTER_BOUND('',#1486,.T.);
#1117=EDGE_LOOP('',(#3865,#3866,#3867,#3868));
#1118=EDGE_LOOP('',(#3869,#3870,#3871,#3872));
#1119=EDGE_LOOP('',(#3873));
#1120=EDGE_LOOP('',(#3874));
#1121=EDGE_LOOP('',(#3875));
#1122=EDGE_LOOP('',(#3876));
#1123=EDGE_LOOP('',(#3877,#3878,#3879,#3880));
#1124=EDGE_LOOP('',(#3881,#3882,#3883,#3884));
#1125=EDGE_LOOP('',(#3885));
#1126=EDGE_LOOP('',(#3886));
#1127=EDGE_LOOP('',(#3887));
#1128=EDGE_LOOP('',(#3888));
#1129=EDGE_LOOP('',(#3889,#3890,#3891,#3892));
#1130=EDGE_LOOP('',(#3893,#3894,#3895,#3896));
#1131=EDGE_LOOP('',(#3897));
#1132=EDGE_LOOP('',(#3898));
#1133=EDGE_LOOP('',(#3899));
#1134=EDGE_LOOP('',(#3900));
#1135=EDGE_LOOP('',(#3901,#3902,#3903,#3904));
#1136=EDGE_LOOP('',(#3905,#3906,#3907,#3908));
#1137=EDGE_LOOP('',(#3909));
#1138=EDGE_LOOP('',(#3910));
#1139=EDGE_LOOP('',(#3911));
#1140=EDGE_LOOP('',(#3912));
#1141=EDGE_LOOP('',(#3913,#3914,#3915,#3916));
#1142=EDGE_LOOP('',(#3917,#3918,#3919,#3920));
#1143=EDGE_LOOP('',(#3921));
#1144=EDGE_LOOP('',(#3922));
#1145=EDGE_LOOP('',(#3923));
#1146=EDGE_LOOP('',(#3924));
#1147=EDGE_LOOP('',(#3925,#3926,#3927,#3928));
#1148=EDGE_LOOP('',(#3929,#3930,#3931,#3932));
#1149=EDGE_LOOP('',(#3933));
#1150=EDGE_LOOP('',(#3934));
#1151=EDGE_LOOP('',(#3935));
#1152=EDGE_LOOP('',(#3936));
#1153=EDGE_LOOP('',(#3937,#3938,#3939,#3940));
#1154=EDGE_LOOP('',(#3941,#3942,#3943,#3944));
#1155=EDGE_LOOP('',(#3945));
#1156=EDGE_LOOP('',(#3946));
#1157=EDGE_LOOP('',(#3947));
#1158=EDGE_LOOP('',(#3948));
#1159=EDGE_LOOP('',(#3949,#3950,#3951,#3952));
#1160=EDGE_LOOP('',(#3953,#3954,#3955,#3956));
#1161=EDGE_LOOP('',(#3957));
#1162=EDGE_LOOP('',(#3958));
#1163=EDGE_LOOP('',(#3959));
#1164=EDGE_LOOP('',(#3960));
#1165=EDGE_LOOP('',(#3961,#3962,#3963,#3964));
#1166=EDGE_LOOP('',(#3965));
#1167=EDGE_LOOP('',(#3966));
#1168=EDGE_LOOP('',(#3967,#3968,#3969,#3970));
#1169=EDGE_LOOP('',(#3971));
#1170=EDGE_LOOP('',(#3972));
#1171=EDGE_LOOP('',(#3973,#3974,#3975,#3976));
#1172=EDGE_LOOP('',(#3977));
#1173=EDGE_LOOP('',(#3978));
#1174=EDGE_LOOP('',(#3979,#3980,#3981,#3982));
#1175=EDGE_LOOP('',(#3983));
#1176=EDGE_LOOP('',(#3984));
#1177=EDGE_LOOP('',(#3985,#3986,#3987,#3988));
#1178=EDGE_LOOP('',(#3989,#3990,#3991,#3992));
#1179=EDGE_LOOP('',(#3993,#3994,#3995,#3996));
#1180=EDGE_LOOP('',(#3997,#3998,#3999,#4000));
#1181=EDGE_LOOP('',(#4001,#4002,#4003,#4004));
#1182=EDGE_LOOP('',(#4005,#4006,#4007,#4008));
#1183=EDGE_LOOP('',(#4009,#4010,#4011,#4012));
#1184=EDGE_LOOP('',(#4013,#4014,#4015,#4016));
#1185=EDGE_LOOP('',(#4017,#4018,#4019,#4020));
#1186=EDGE_LOOP('',(#4021));
#1187=EDGE_LOOP('',(#4022));
#1188=EDGE_LOOP('',(#4023));
#1189=EDGE_LOOP('',(#4024));
#1190=EDGE_LOOP('',(#4025,#4026,#4027,#4028));
#1191=EDGE_LOOP('',(#4029));
#1192=EDGE_LOOP('',(#4030));
#1193=EDGE_LOOP('',(#4031));
#1194=EDGE_LOOP('',(#4032));
#1195=EDGE_LOOP('',(#4033,#4034,#4035,#4036));
#1196=EDGE_LOOP('',(#4037,#4038,#4039,#4040));
#1197=EDGE_LOOP('',(#4041,#4042,#4043,#4044));
#1198=EDGE_LOOP('',(#4045,#4046,#4047,#4048));
#1199=EDGE_LOOP('',(#4049,#4050,#4051,#4052));
#1200=EDGE_LOOP('',(#4053,#4054,#4055,#4056));
#1201=EDGE_LOOP('',(#4057,#4058,#4059,#4060));
#1202=EDGE_LOOP('',(#4061,#4062,#4063,#4064,#4065,#4066,#4067,#4068,#4069,
#4070,#4071,#4072));
#1203=EDGE_LOOP('',(#4073));
#1204=EDGE_LOOP('',(#4074));
#1205=EDGE_LOOP('',(#4075));
#1206=EDGE_LOOP('',(#4076));
#1207=EDGE_LOOP('',(#4077,#4078,#4079,#4080));
#1208=EDGE_LOOP('',(#4081,#4082,#4083,#4084));
#1209=EDGE_LOOP('',(#4085,#4086,#4087,#4088));
#1210=EDGE_LOOP('',(#4089,#4090,#4091,#4092));
#1211=EDGE_LOOP('',(#4093,#4094,#4095,#4096));
#1212=EDGE_LOOP('',(#4097,#4098,#4099,#4100));
#1213=EDGE_LOOP('',(#4101,#4102,#4103,#4104));
#1214=EDGE_LOOP('',(#4105,#4106,#4107,#4108));
#1215=EDGE_LOOP('',(#4109,#4110,#4111,#4112));
#1216=EDGE_LOOP('',(#4113,#4114,#4115,#4116,#4117,#4118,#4119,#4120,#4121,
#4122,#4123,#4124));
#1217=EDGE_LOOP('',(#4125));
#1218=EDGE_LOOP('',(#4126));
#1219=EDGE_LOOP('',(#4127));
#1220=EDGE_LOOP('',(#4128));
#1221=EDGE_LOOP('',(#4129,#4130,#4131,#4132));
#1222=EDGE_LOOP('',(#4133,#4134,#4135,#4136));
#1223=EDGE_LOOP('',(#4137,#4138,#4139,#4140));
#1224=EDGE_LOOP('',(#4141,#4142,#4143,#4144));
#1225=EDGE_LOOP('',(#4145));
#1226=EDGE_LOOP('',(#4146,#4147,#4148,#4149));
#1227=EDGE_LOOP('',(#4150,#4151,#4152,#4153));
#1228=EDGE_LOOP('',(#4154));
#1229=EDGE_LOOP('',(#4155,#4156,#4157,#4158));
#1230=EDGE_LOOP('',(#4159));
#1231=EDGE_LOOP('',(#4160));
#1232=EDGE_LOOP('',(#4161,#4162,#4163,#4164));
#1233=EDGE_LOOP('',(#4165,#4166,#4167,#4168));
#1234=EDGE_LOOP('',(#4169));
#1235=EDGE_LOOP('',(#4170));
#1236=EDGE_LOOP('',(#4171,#4172,#4173,#4174,#4175,#4176));
#1237=EDGE_LOOP('',(#4177,#4178,#4179,#4180,#4181,#4182));
#1238=EDGE_LOOP('',(#4183,#4184,#4185,#4186));
#1239=EDGE_LOOP('',(#4187,#4188,#4189,#4190));
#1240=EDGE_LOOP('',(#4191,#4192,#4193,#4194));
#1241=EDGE_LOOP('',(#4195,#4196,#4197,#4198));
#1242=EDGE_LOOP('',(#4199));
#1243=EDGE_LOOP('',(#4200,#4201,#4202,#4203));
#1244=EDGE_LOOP('',(#4204,#4205,#4206,#4207));
#1245=EDGE_LOOP('',(#4208));
#1246=EDGE_LOOP('',(#4209,#4210,#4211,#4212));
#1247=EDGE_LOOP('',(#4213));
#1248=EDGE_LOOP('',(#4214));
#1249=EDGE_LOOP('',(#4215,#4216,#4217,#4218));
#1250=EDGE_LOOP('',(#4219,#4220,#4221,#4222));
#1251=EDGE_LOOP('',(#4223));
#1252=EDGE_LOOP('',(#4224));
#1253=EDGE_LOOP('',(#4225,#4226,#4227,#4228,#4229,#4230));
#1254=EDGE_LOOP('',(#4231,#4232,#4233,#4234,#4235,#4236));
#1255=EDGE_LOOP('',(#4237,#4238,#4239,#4240));
#1256=EDGE_LOOP('',(#4241,#4242,#4243,#4244));
#1257=EDGE_LOOP('',(#4245,#4246,#4247,#4248));
#1258=EDGE_LOOP('',(#4249,#4250,#4251,#4252));
#1259=EDGE_LOOP('',(#4253,#4254,#4255,#4256));
#1260=EDGE_LOOP('',(#4257,#4258,#4259,#4260));
#1261=EDGE_LOOP('',(#4261,#4262,#4263,#4264));
#1262=EDGE_LOOP('',(#4265));
#1263=EDGE_LOOP('',(#4266));
#1264=EDGE_LOOP('',(#4267,#4268,#4269,#4270));
#1265=EDGE_LOOP('',(#4271));
#1266=EDGE_LOOP('',(#4272));
#1267=EDGE_LOOP('',(#4273,#4274,#4275,#4276,#4277,#4278,#4279,#4280,#4281,
#4282));
#1268=EDGE_LOOP('',(#4283,#4284));
#1269=EDGE_LOOP('',(#4285,#4286,#4287,#4288,#4289,#4290,#4291,#4292,#4293,
#4294));
#1270=EDGE_LOOP('',(#4295,#4296));
#1271=EDGE_LOOP('',(#4297,#4298,#4299,#4300,#4301,#4302,#4303,#4304));
#1272=EDGE_LOOP('',(#4305,#4306,#4307,#4308,#4309,#4310,#4311,#4312));
#1273=EDGE_LOOP('',(#4313,#4314,#4315,#4316,#4317,#4318,#4319,#4320,#4321));
#1274=EDGE_LOOP('',(#4322,#4323));
#1275=EDGE_LOOP('',(#4324,#4325,#4326,#4327,#4328,#4329,#4330,#4331,#4332));
#1276=EDGE_LOOP('',(#4333,#4334));
#1277=EDGE_LOOP('',(#4335,#4336,#4337,#4338,#4339,#4340,#4341));
#1278=EDGE_LOOP('',(#4342,#4343,#4344,#4345,#4346,#4347));
#1279=EDGE_LOOP('',(#4348,#4349,#4350,#4351));
#1280=EDGE_LOOP('',(#4352,#4353,#4354,#4355));
#1281=EDGE_LOOP('',(#4356,#4357,#4358,#4359));
#1282=EDGE_LOOP('',(#4360,#4361,#4362,#4363));
#1283=EDGE_LOOP('',(#4364,#4365,#4366,#4367));
#1284=EDGE_LOOP('',(#4368));
#1285=EDGE_LOOP('',(#4369));
#1286=EDGE_LOOP('',(#4370,#4371,#4372,#4373));
#1287=EDGE_LOOP('',(#4374,#4375,#4376,#4377));
#1288=EDGE_LOOP('',(#4378,#4379,#4380,#4381));
#1289=EDGE_LOOP('',(#4382,#4383,#4384,#4385));
#1290=EDGE_LOOP('',(#4386,#4387,#4388,#4389));
#1291=EDGE_LOOP('',(#4390,#4391,#4392,#4393));
#1292=EDGE_LOOP('',(#4394,#4395,#4396,#4397));
#1293=EDGE_LOOP('',(#4398,#4399,#4400,#4401));
#1294=EDGE_LOOP('',(#4402,#4403,#4404,#4405));
#1295=EDGE_LOOP('',(#4406));
#1296=EDGE_LOOP('',(#4407));
#1297=EDGE_LOOP('',(#4408,#4409,#4410,#4411));
#1298=EDGE_LOOP('',(#4412,#4413,#4414,#4415));
#1299=EDGE_LOOP('',(#4416,#4417,#4418,#4419));
#1300=EDGE_LOOP('',(#4420,#4421,#4422,#4423));
#1301=EDGE_LOOP('',(#4424,#4425,#4426,#4427));
#1302=EDGE_LOOP('',(#4428,#4429,#4430,#4431));
#1303=EDGE_LOOP('',(#4432,#4433,#4434,#4435));
#1304=EDGE_LOOP('',(#4436,#4437,#4438,#4439));
#1305=EDGE_LOOP('',(#4440,#4441,#4442,#4443));
#1306=EDGE_LOOP('',(#4444));
#1307=EDGE_LOOP('',(#4445));
#1308=EDGE_LOOP('',(#4446,#4447,#4448,#4449));
#1309=EDGE_LOOP('',(#4450,#4451,#4452,#4453));
#1310=EDGE_LOOP('',(#4454,#4455,#4456,#4457));
#1311=EDGE_LOOP('',(#4458,#4459,#4460,#4461));
#1312=EDGE_LOOP('',(#4462,#4463,#4464,#4465));
#1313=EDGE_LOOP('',(#4466,#4467,#4468,#4469));
#1314=EDGE_LOOP('',(#4470,#4471,#4472,#4473));
#1315=EDGE_LOOP('',(#4474,#4475,#4476,#4477));
#1316=EDGE_LOOP('',(#4478,#4479,#4480,#4481));
#1317=EDGE_LOOP('',(#4482));
#1318=EDGE_LOOP('',(#4483));
#1319=EDGE_LOOP('',(#4484,#4485,#4486,#4487));
#1320=EDGE_LOOP('',(#4488,#4489,#4490,#4491));
#1321=EDGE_LOOP('',(#4492,#4493,#4494,#4495));
#1322=EDGE_LOOP('',(#4496,#4497,#4498,#4499));
#1323=EDGE_LOOP('',(#4500,#4501,#4502,#4503,#4504));
#1324=EDGE_LOOP('',(#4505,#4506,#4507,#4508));
#1325=EDGE_LOOP('',(#4509,#4510,#4511,#4512));
#1326=EDGE_LOOP('',(#4513,#4514,#4515,#4516));
#1327=EDGE_LOOP('',(#4517,#4518,#4519,#4520));
#1328=EDGE_LOOP('',(#4521,#4522,#4523,#4524));
#1329=EDGE_LOOP('',(#4525,#4526,#4527,#4528));
#1330=EDGE_LOOP('',(#4529,#4530,#4531,#4532));
#1331=EDGE_LOOP('',(#4533,#4534,#4535,#4536));
#1332=EDGE_LOOP('',(#4537,#4538,#4539,#4540,#4541,#4542,#4543,#4544,#4545,
#4546,#4547,#4548,#4549,#4550,#4551,#4552,#4553,#4554,#4555,#4556,#4557,
#4558,#4559,#4560,#4561,#4562,#4563,#4564,#4565,#4566,#4567,#4568,#4569,
#4570,#4571,#4572,#4573,#4574,#4575,#4576,#4577,#4578,#4579,#4580));
#1333=EDGE_LOOP('',(#4581));
#1334=EDGE_LOOP('',(#4582,#4583,#4584,#4585,#4586,#4587,#4588,#4589,#4590,
#4591,#4592,#4593,#4594,#4595,#4596,#4597,#4598,#4599,#4600,#4601,#4602,
#4603,#4604,#4605,#4606,#4607,#4608,#4609,#4610,#4611,#4612,#4613,#4614,
#4615,#4616,#4617,#4618,#4619,#4620,#4621,#4622,#4623,#4624,#4625));
#1335=EDGE_LOOP('',(#4626));
#1336=EDGE_LOOP('',(#4627,#4628,#4629,#4630,#4631,#4632,#4633,#4634,#4635,
#4636,#4637,#4638,#4639,#4640,#4641,#4642,#4643,#4644,#4645,#4646,#4647,
#4648,#4649,#4650,#4651,#4652,#4653,#4654,#4655,#4656,#4657,#4658,#4659,
#4660,#4661,#4662,#4663,#4664,#4665,#4666,#4667,#4668,#4669,#4670));
#1337=EDGE_LOOP('',(#4671));
#1338=EDGE_LOOP('',(#4672,#4673,#4674,#4675));
#1339=EDGE_LOOP('',(#4676,#4677,#4678,#4679));
#1340=EDGE_LOOP('',(#4680,#4681,#4682,#4683));
#1341=EDGE_LOOP('',(#4684,#4685,#4686,#4687));
#1342=EDGE_LOOP('',(#4688,#4689,#4690,#4691));
#1343=EDGE_LOOP('',(#4692,#4693,#4694,#4695));
#1344=EDGE_LOOP('',(#4696,#4697,#4698,#4699));
#1345=EDGE_LOOP('',(#4700,#4701,#4702,#4703));
#1346=EDGE_LOOP('',(#4704,#4705,#4706,#4707));
#1347=EDGE_LOOP('',(#4708,#4709,#4710,#4711));
#1348=EDGE_LOOP('',(#4712,#4713,#4714,#4715));
#1349=EDGE_LOOP('',(#4716,#4717,#4718,#4719));
#1350=EDGE_LOOP('',(#4720,#4721,#4722,#4723));
#1351=EDGE_LOOP('',(#4724,#4725,#4726,#4727));
#1352=EDGE_LOOP('',(#4728,#4729,#4730,#4731));
#1353=EDGE_LOOP('',(#4732,#4733,#4734,#4735));
#1354=EDGE_LOOP('',(#4736,#4737,#4738,#4739));
#1355=EDGE_LOOP('',(#4740,#4741,#4742,#4743));
#1356=EDGE_LOOP('',(#4744,#4745,#4746,#4747));
#1357=EDGE_LOOP('',(#4748,#4749,#4750,#4751));
#1358=EDGE_LOOP('',(#4752,#4753,#4754,#4755));
#1359=EDGE_LOOP('',(#4756,#4757,#4758,#4759));
#1360=EDGE_LOOP('',(#4760,#4761,#4762,#4763));
#1361=EDGE_LOOP('',(#4764,#4765,#4766,#4767));
#1362=EDGE_LOOP('',(#4768,#4769,#4770,#4771));
#1363=EDGE_LOOP('',(#4772,#4773,#4774,#4775));
#1364=EDGE_LOOP('',(#4776,#4777,#4778,#4779));
#1365=EDGE_LOOP('',(#4780,#4781,#4782,#4783));
#1366=EDGE_LOOP('',(#4784,#4785,#4786,#4787));
#1367=EDGE_LOOP('',(#4788,#4789,#4790,#4791));
#1368=EDGE_LOOP('',(#4792,#4793,#4794,#4795));
#1369=EDGE_LOOP('',(#4796,#4797,#4798,#4799));
#1370=EDGE_LOOP('',(#4800,#4801,#4802,#4803));
#1371=EDGE_LOOP('',(#4804,#4805,#4806,#4807));
#1372=EDGE_LOOP('',(#4808,#4809,#4810,#4811));
#1373=EDGE_LOOP('',(#4812,#4813,#4814,#4815));
#1374=EDGE_LOOP('',(#4816,#4817,#4818,#4819));
#1375=EDGE_LOOP('',(#4820,#4821,#4822,#4823));
#1376=EDGE_LOOP('',(#4824,#4825,#4826,#4827));
#1377=EDGE_LOOP('',(#4828,#4829,#4830,#4831));
#1378=EDGE_LOOP('',(#4832,#4833,#4834,#4835));
#1379=EDGE_LOOP('',(#4836,#4837,#4838,#4839));
#1380=EDGE_LOOP('',(#4840,#4841,#4842,#4843));
#1381=EDGE_LOOP('',(#4844,#4845,#4846,#4847));
#1382=EDGE_LOOP('',(#4848,#4849,#4850,#4851));
#1383=EDGE_LOOP('',(#4852,#4853,#4854,#4855,#4856,#4857,#4858,#4859,#4860,
#4861,#4862,#4863,#4864,#4865,#4866,#4867,#4868,#4869,#4870,#4871,#4872,
#4873,#4874,#4875,#4876,#4877,#4878,#4879,#4880,#4881,#4882,#4883,#4884,
#4885,#4886,#4887,#4888,#4889,#4890,#4891,#4892,#4893,#4894,#4895));
#1384=EDGE_LOOP('',(#4896));
#1385=EDGE_LOOP('',(#4897,#4898,#4899,#4900));
#1386=EDGE_LOOP('',(#4901,#4902,#4903,#4904));
#1387=EDGE_LOOP('',(#4905,#4906,#4907,#4908));
#1388=EDGE_LOOP('',(#4909,#4910,#4911,#4912));
#1389=EDGE_LOOP('',(#4913,#4914,#4915,#4916));
#1390=EDGE_LOOP('',(#4917,#4918,#4919,#4920));
#1391=EDGE_LOOP('',(#4921,#4922,#4923,#4924,#4925,#4926));
#1392=EDGE_LOOP('',(#4927,#4928,#4929,#4930,#4931,#4932));
#1393=EDGE_LOOP('',(#4933));
#1394=EDGE_LOOP('',(#4934));
#1395=EDGE_LOOP('',(#4935,#4936,#4937,#4938));
#1396=EDGE_LOOP('',(#4939));
#1397=EDGE_LOOP('',(#4940));
#1398=EDGE_LOOP('',(#4941,#4942,#4943,#4944));
#1399=EDGE_LOOP('',(#4945,#4946,#4947,#4948));
#1400=EDGE_LOOP('',(#4949,#4950,#4951,#4952));
#1401=EDGE_LOOP('',(#4953));
#1402=EDGE_LOOP('',(#4954));
#1403=EDGE_LOOP('',(#4955,#4956,#4957,#4958));
#1404=EDGE_LOOP('',(#4959,#4960,#4961,#4962));
#1405=EDGE_LOOP('',(#4963));
#1406=EDGE_LOOP('',(#4964,#4965,#4966,#4967));
#1407=EDGE_LOOP('',(#4968,#4969,#4970,#4971));
#1408=EDGE_LOOP('',(#4972,#4973,#4974,#4975));
#1409=EDGE_LOOP('',(#4976));
#1410=EDGE_LOOP('',(#4977));
#1411=EDGE_LOOP('',(#4978,#4979,#4980,#4981));
#1412=EDGE_LOOP('',(#4982,#4983,#4984,#4985));
#1413=EDGE_LOOP('',(#4986,#4987,#4988,#4989));
#1414=EDGE_LOOP('',(#4990));
#1415=EDGE_LOOP('',(#4991,#4992,#4993,#4994));
#1416=EDGE_LOOP('',(#4995,#4996,#4997,#4998));
#1417=EDGE_LOOP('',(#4999,#5000,#5001,#5002));
#1418=EDGE_LOOP('',(#5003,#5004,#5005,#5006));
#1419=EDGE_LOOP('',(#5007,#5008,#5009,#5010));
#1420=EDGE_LOOP('',(#5011,#5012,#5013,#5014));
#1421=EDGE_LOOP('',(#5015,#5016,#5017,#5018,#5019,#5020));
#1422=EDGE_LOOP('',(#5021,#5022,#5023,#5024,#5025,#5026));
#1423=EDGE_LOOP('',(#5027,#5028,#5029,#5030));
#1424=EDGE_LOOP('',(#5031,#5032,#5033,#5034));
#1425=EDGE_LOOP('',(#5035,#5036,#5037,#5038));
#1426=EDGE_LOOP('',(#5039));
#1427=EDGE_LOOP('',(#5040,#5041,#5042,#5043,#5044,#5045,#5046,#5047,#5048,
#5049));
#1428=EDGE_LOOP('',(#5050,#5051,#5052,#5053));
#1429=EDGE_LOOP('',(#5054,#5055,#5056,#5057));
#1430=EDGE_LOOP('',(#5058,#5059,#5060,#5061,#5062,#5063,#5064,#5065,#5066,
#5067));
#1431=EDGE_LOOP('',(#5068,#5069,#5070,#5071));
#1432=EDGE_LOOP('',(#5072,#5073,#5074,#5075,#5076,#5077));
#1433=EDGE_LOOP('',(#5078,#5079,#5080,#5081,#5082,#5083,#5084,#5085));
#1434=EDGE_LOOP('',(#5086,#5087,#5088,#5089,#5090));
#1435=EDGE_LOOP('',(#5091,#5092,#5093,#5094));
#1436=EDGE_LOOP('',(#5095,#5096,#5097,#5098,#5099,#5100));
#1437=EDGE_LOOP('',(#5101,#5102,#5103,#5104));
#1438=EDGE_LOOP('',(#5105,#5106,#5107,#5108));
#1439=EDGE_LOOP('',(#5109,#5110,#5111,#5112));
#1440=EDGE_LOOP('',(#5113));
#1441=EDGE_LOOP('',(#5114));
#1442=EDGE_LOOP('',(#5115,#5116,#5117,#5118));
#1443=EDGE_LOOP('',(#5119));
#1444=EDGE_LOOP('',(#5120));
#1445=EDGE_LOOP('',(#5121,#5122,#5123,#5124));
#1446=EDGE_LOOP('',(#5125,#5126,#5127,#5128));
#1447=EDGE_LOOP('',(#5129,#5130,#5131,#5132));
#1448=EDGE_LOOP('',(#5133,#5134,#5135,#5136));
#1449=EDGE_LOOP('',(#5137,#5138,#5139,#5140));
#1450=EDGE_LOOP('',(#5141,#5142,#5143,#5144));
#1451=EDGE_LOOP('',(#5145,#5146,#5147,#5148,#5149,#5150));
#1452=EDGE_LOOP('',(#5151,#5152,#5153,#5154,#5155,#5156));
#1453=EDGE_LOOP('',(#5157));
#1454=EDGE_LOOP('',(#5158));
#1455=EDGE_LOOP('',(#5159,#5160,#5161,#5162));
#1456=EDGE_LOOP('',(#5163,#5164,#5165,#5166));
#1457=EDGE_LOOP('',(#5167,#5168,#5169,#5170));
#1458=EDGE_LOOP('',(#5171));
#1459=EDGE_LOOP('',(#5172));
#1460=EDGE_LOOP('',(#5173,#5174,#5175,#5176));
#1461=EDGE_LOOP('',(#5177,#5178,#5179,#5180));
#1462=EDGE_LOOP('',(#5181,#5182,#5183,#5184));
#1463=EDGE_LOOP('',(#5185,#5186,#5187,#5188));
#1464=EDGE_LOOP('',(#5189));
#1465=EDGE_LOOP('',(#5190));
#1466=EDGE_LOOP('',(#5191,#5192,#5193,#5194));
#1467=EDGE_LOOP('',(#5195));
#1468=EDGE_LOOP('',(#5196));
#1469=EDGE_LOOP('',(#5197));
#1470=EDGE_LOOP('',(#5198,#5199,#5200,#5201));
#1471=EDGE_LOOP('',(#5202,#5203,#5204,#5205));
#1472=EDGE_LOOP('',(#5206,#5207,#5208,#5209));
#1473=EDGE_LOOP('',(#5210));
#1474=EDGE_LOOP('',(#5211));
#1475=EDGE_LOOP('',(#5212,#5213,#5214,#5215));
#1476=EDGE_LOOP('',(#5216,#5217,#5218,#5219));
#1477=EDGE_LOOP('',(#5220,#5221,#5222,#5223));
#1478=EDGE_LOOP('',(#5224));
#1479=EDGE_LOOP('',(#5225,#5226,#5227,#5228));
#1480=EDGE_LOOP('',(#5229,#5230,#5231,#5232));
#1481=EDGE_LOOP('',(#5233,#5234,#5235,#5236));
#1482=EDGE_LOOP('',(#5237,#5238,#5239,#5240));
#1483=EDGE_LOOP('',(#5241,#5242,#5243,#5244));
#1484=EDGE_LOOP('',(#5245,#5246,#5247,#5248));
#1485=EDGE_LOOP('',(#5249,#5250,#5251,#5252,#5253,#5254));
#1486=EDGE_LOOP('',(#5255,#5256,#5257,#5258,#5259,#5260));
#1487=LINE('',#8064,#2031);
#1488=LINE('',#8070,#2032);
#1489=LINE('',#8079,#2033);
#1490=LINE('',#8085,#2034);
#1491=LINE('',#8094,#2035);
#1492=LINE('',#8100,#2036);
#1493=LINE('',#8109,#2037);
#1494=LINE('',#8115,#2038);
#1495=LINE('',#8124,#2039);
#1496=LINE('',#8130,#2040);
#1497=LINE('',#8139,#2041);
#1498=LINE('',#8145,#2042);
#1499=LINE('',#8154,#2043);
#1500=LINE('',#8160,#2044);
#1501=LINE('',#8169,#2045);
#1502=LINE('',#8175,#2046);
#1503=LINE('',#8184,#2047);
#1504=LINE('',#8193,#2048);
#1505=LINE('',#8202,#2049);
#1506=LINE('',#8211,#2050);
#1507=LINE('',#8219,#2051);
#1508=LINE('',#8223,#2052);
#1509=LINE('',#8227,#2053);
#1510=LINE('',#8231,#2054);
#1511=LINE('',#8235,#2055);
#1512=LINE('',#8237,#2056);
#1513=LINE('',#8239,#2057);
#1514=LINE('',#8240,#2058);
#1515=LINE('',#8243,#2059);
#1516=LINE('',#8245,#2060);
#1517=LINE('',#8246,#2061);
#1518=LINE('',#8249,#2062);
#1519=LINE('',#8251,#2063);
#1520=LINE('',#8252,#2064);
#1521=LINE('',#8254,#2065);
#1522=LINE('',#8255,#2066);
#1523=LINE('',#8263,#2067);
#1524=LINE('',#8269,#2068);
#1525=LINE('',#8275,#2069);
#1526=LINE('',#8281,#2070);
#1527=LINE('',#8286,#2071);
#1528=LINE('',#8288,#2072);
#1529=LINE('',#8290,#2073);
#1530=LINE('',#8291,#2074);
#1531=LINE('',#8294,#2075);
#1532=LINE('',#8296,#2076);
#1533=LINE('',#8297,#2077);
#1534=LINE('',#8300,#2078);
#1535=LINE('',#8302,#2079);
#1536=LINE('',#8303,#2080);
#1537=LINE('',#8306,#2081);
#1538=LINE('',#8308,#2082);
#1539=LINE('',#8310,#2083);
#1540=LINE('',#8312,#2084);
#1541=LINE('',#8314,#2085);
#1542=LINE('',#8316,#2086);
#1543=LINE('',#8318,#2087);
#1544=LINE('',#8320,#2088);
#1545=LINE('',#8321,#2089);
#1546=LINE('',#8325,#2090);
#1547=LINE('',#8326,#2091);
#1548=LINE('',#8327,#2092);
#1549=LINE('',#8329,#2093);
#1550=LINE('',#8332,#2094);
#1551=LINE('',#8333,#2095);
#1552=LINE('',#8337,#2096);
#1553=LINE('',#8338,#2097);
#1554=LINE('',#8339,#2098);
#1555=LINE('',#8342,#2099);
#1556=LINE('',#8343,#2100);
#1557=LINE('',#8345,#2101);
#1558=LINE('',#8348,#2102);
#1559=LINE('',#8349,#2103);
#1560=LINE('',#8352,#2104);
#1561=LINE('',#8353,#2105);
#1562=LINE('',#8355,#2106);
#1563=LINE('',#8362,#2107);
#1564=LINE('',#8368,#2108);
#1565=LINE('',#8374,#2109);
#1566=LINE('',#8379,#2110);
#1567=LINE('',#8381,#2111);
#1568=LINE('',#8383,#2112);
#1569=LINE('',#8384,#2113);
#1570=LINE('',#8387,#2114);
#1571=LINE('',#8389,#2115);
#1572=LINE('',#8390,#2116);
#1573=LINE('',#8393,#2117);
#1574=LINE('',#8395,#2118);
#1575=LINE('',#8396,#2119);
#1576=LINE('',#8399,#2120);
#1577=LINE('',#8401,#2121);
#1578=LINE('',#8402,#2122);
#1579=LINE('',#8405,#2123);
#1580=LINE('',#8407,#2124);
#1581=LINE('',#8408,#2125);
#1582=LINE('',#8410,#2126);
#1583=LINE('',#8411,#2127);
#1584=LINE('',#8419,#2128);
#1585=LINE('',#8425,#2129);
#1586=LINE('',#8431,#2130);
#1587=LINE('',#8436,#2131);
#1588=LINE('',#8438,#2132);
#1589=LINE('',#8440,#2133);
#1590=LINE('',#8441,#2134);
#1591=LINE('',#8444,#2135);
#1592=LINE('',#8446,#2136);
#1593=LINE('',#8447,#2137);
#1594=LINE('',#8450,#2138);
#1595=LINE('',#8452,#2139);
#1596=LINE('',#8453,#2140);
#1597=LINE('',#8456,#2141);
#1598=LINE('',#8458,#2142);
#1599=LINE('',#8459,#2143);
#1600=LINE('',#8462,#2144);
#1601=LINE('',#8464,#2145);
#1602=LINE('',#8465,#2146);
#1603=LINE('',#8467,#2147);
#1604=LINE('',#8468,#2148);
#1605=LINE('',#8476,#2149);
#1606=LINE('',#8482,#2150);
#1607=LINE('',#8487,#2151);
#1608=LINE('',#8489,#2152);
#1609=LINE('',#8491,#2153);
#1610=LINE('',#8492,#2154);
#1611=LINE('',#8495,#2155);
#1612=LINE('',#8497,#2156);
#1613=LINE('',#8498,#2157);
#1614=LINE('',#8501,#2158);
#1615=LINE('',#8503,#2159);
#1616=LINE('',#8504,#2160);
#1617=LINE('',#8506,#2161);
#1618=LINE('',#8507,#2162);
#1619=LINE('',#8515,#2163);
#1620=LINE('',#8543,#2164);
#1621=LINE('',#8620,#2165);
#1622=LINE('',#8648,#2166);
#1623=LINE('',#8722,#2167);
#1624=LINE('',#8758,#2168);
#1625=LINE('',#8775,#2169);
#1626=LINE('',#8800,#2170);
#1627=LINE('',#8831,#2171);
#1628=LINE('',#8856,#2172);
#1629=LINE('',#8930,#2173);
#1630=LINE('',#8934,#2174);
#1631=LINE('',#8938,#2175);
#1632=LINE('',#8940,#2176);
#1633=LINE('',#8942,#2177);
#1634=LINE('',#8943,#2178);
#1635=LINE('',#8946,#2179);
#1636=LINE('',#8948,#2180);
#1637=LINE('',#8949,#2181);
#1638=LINE('',#8952,#2182);
#1639=LINE('',#8954,#2183);
#1640=LINE('',#8955,#2184);
#1641=LINE('',#8958,#2185);
#1642=LINE('',#8960,#2186);
#1643=LINE('',#8961,#2187);
#1644=LINE('',#8964,#2188);
#1645=LINE('',#8966,#2189);
#1646=LINE('',#8967,#2190);
#1647=LINE('',#8970,#2191);
#1648=LINE('',#8972,#2192);
#1649=LINE('',#8973,#2193);
#1650=LINE('',#8976,#2194);
#1651=LINE('',#8978,#2195);
#1652=LINE('',#8979,#2196);
#1653=LINE('',#8982,#2197);
#1654=LINE('',#8984,#2198);
#1655=LINE('',#8985,#2199);
#1656=LINE('',#8988,#2200);
#1657=LINE('',#8990,#2201);
#1658=LINE('',#8991,#2202);
#1659=LINE('',#8995,#2203);
#1660=LINE('',#8997,#2204);
#1661=LINE('',#8999,#2205);
#1662=LINE('',#9000,#2206);
#1663=LINE('',#9003,#2207);
#1664=LINE('',#9005,#2208);
#1665=LINE('',#9006,#2209);
#1666=LINE('',#9009,#2210);
#1667=LINE('',#9011,#2211);
#1668=LINE('',#9012,#2212);
#1669=LINE('',#9015,#2213);
#1670=LINE('',#9017,#2214);
#1671=LINE('',#9018,#2215);
#1672=LINE('',#9021,#2216);
#1673=LINE('',#9023,#2217);
#1674=LINE('',#9024,#2218);
#1675=LINE('',#9027,#2219);
#1676=LINE('',#9029,#2220);
#1677=LINE('',#9030,#2221);
#1678=LINE('',#9033,#2222);
#1679=LINE('',#9035,#2223);
#1680=LINE('',#9036,#2224);
#1681=LINE('',#9039,#2225);
#1682=LINE('',#9041,#2226);
#1683=LINE('',#9042,#2227);
#1684=LINE('',#9045,#2228);
#1685=LINE('',#9047,#2229);
#1686=LINE('',#9048,#2230);
#1687=LINE('',#9052,#2231);
#1688=LINE('',#9054,#2232);
#1689=LINE('',#9056,#2233);
#1690=LINE('',#9057,#2234);
#1691=LINE('',#9060,#2235);
#1692=LINE('',#9062,#2236);
#1693=LINE('',#9063,#2237);
#1694=LINE('',#9066,#2238);
#1695=LINE('',#9068,#2239);
#1696=LINE('',#9069,#2240);
#1697=LINE('',#9072,#2241);
#1698=LINE('',#9074,#2242);
#1699=LINE('',#9075,#2243);
#1700=LINE('',#9078,#2244);
#1701=LINE('',#9080,#2245);
#1702=LINE('',#9081,#2246);
#1703=LINE('',#9084,#2247);
#1704=LINE('',#9086,#2248);
#1705=LINE('',#9087,#2249);
#1706=LINE('',#9090,#2250);
#1707=LINE('',#9092,#2251);
#1708=LINE('',#9093,#2252);
#1709=LINE('',#9096,#2253);
#1710=LINE('',#9098,#2254);
#1711=LINE('',#9099,#2255);
#1712=LINE('',#9102,#2256);
#1713=LINE('',#9104,#2257);
#1714=LINE('',#9105,#2258);
#1715=LINE('',#9109,#2259);
#1716=LINE('',#9111,#2260);
#1717=LINE('',#9113,#2261);
#1718=LINE('',#9114,#2262);
#1719=LINE('',#9117,#2263);
#1720=LINE('',#9119,#2264);
#1721=LINE('',#9120,#2265);
#1722=LINE('',#9123,#2266);
#1723=LINE('',#9125,#2267);
#1724=LINE('',#9126,#2268);
#1725=LINE('',#9129,#2269);
#1726=LINE('',#9131,#2270);
#1727=LINE('',#9132,#2271);
#1728=LINE('',#9135,#2272);
#1729=LINE('',#9137,#2273);
#1730=LINE('',#9138,#2274);
#1731=LINE('',#9141,#2275);
#1732=LINE('',#9143,#2276);
#1733=LINE('',#9144,#2277);
#1734=LINE('',#9147,#2278);
#1735=LINE('',#9149,#2279);
#1736=LINE('',#9150,#2280);
#1737=LINE('',#9153,#2281);
#1738=LINE('',#9155,#2282);
#1739=LINE('',#9156,#2283);
#1740=LINE('',#9159,#2284);
#1741=LINE('',#9161,#2285);
#1742=LINE('',#9162,#2286);
#1743=LINE('',#9165,#2287);
#1744=LINE('',#9169,#2288);
#1745=LINE('',#9171,#2289);
#1746=LINE('',#9172,#2290);
#1747=LINE('',#9175,#2291);
#1748=LINE('',#9177,#2292);
#1749=LINE('',#9178,#2293);
#1750=LINE('',#9180,#2294);
#1751=LINE('',#9181,#2295);
#1752=LINE('',#9184,#2296);
#1753=LINE('',#9186,#2297);
#1754=LINE('',#9187,#2298);
#1755=LINE('',#9189,#2299);
#1756=LINE('',#9190,#2300);
#1757=LINE('',#9193,#2301);
#1758=LINE('',#9195,#2302);
#1759=LINE('',#9196,#2303);
#1760=LINE('',#9198,#2304);
#1761=LINE('',#9199,#2305);
#1762=LINE('',#9201,#2306);
#1763=LINE('',#9202,#2307);
#1764=LINE('',#9209,#2308);
#1765=LINE('',#9211,#2309);
#1766=LINE('',#9213,#2310);
#1767=LINE('',#9215,#2311);
#1768=LINE('',#9217,#2312);
#1769=LINE('',#9219,#2313);
#1770=LINE('',#9221,#2314);
#1771=LINE('',#9223,#2315);
#1772=LINE('',#9225,#2316);
#1773=LINE('',#9227,#2317);
#1774=LINE('',#9229,#2318);
#1775=LINE('',#9231,#2319);
#1776=LINE('',#9233,#2320);
#1777=LINE('',#9235,#2321);
#1778=LINE('',#9237,#2322);
#1779=LINE('',#9239,#2323);
#1780=LINE('',#9241,#2324);
#1781=LINE('',#9243,#2325);
#1782=LINE('',#9245,#2326);
#1783=LINE('',#9247,#2327);
#1784=LINE('',#9249,#2328);
#1785=LINE('',#9251,#2329);
#1786=LINE('',#9253,#2330);
#1787=LINE('',#9255,#2331);
#1788=LINE('',#9257,#2332);
#1789=LINE('',#9259,#2333);
#1790=LINE('',#9261,#2334);
#1791=LINE('',#9263,#2335);
#1792=LINE('',#9265,#2336);
#1793=LINE('',#9267,#2337);
#1794=LINE('',#9269,#2338);
#1795=LINE('',#9271,#2339);
#1796=LINE('',#9273,#2340);
#1797=LINE('',#9275,#2341);
#1798=LINE('',#9277,#2342);
#1799=LINE('',#9279,#2343);
#1800=LINE('',#9281,#2344);
#1801=LINE('',#9283,#2345);
#1802=LINE('',#9285,#2346);
#1803=LINE('',#9287,#2347);
#1804=LINE('',#9289,#2348);
#1805=LINE('',#9291,#2349);
#1806=LINE('',#9293,#2350);
#1807=LINE('',#9294,#2351);
#1808=LINE('',#9299,#2352);
#1809=LINE('',#9301,#2353);
#1810=LINE('',#9302,#2354);
#1811=LINE('',#9305,#2355);
#1812=LINE('',#9306,#2356);
#1813=LINE('',#9309,#2357);
#1814=LINE('',#9310,#2358);
#1815=LINE('',#9313,#2359);
#1816=LINE('',#9314,#2360);
#1817=LINE('',#9317,#2361);
#1818=LINE('',#9318,#2362);
#1819=LINE('',#9321,#2363);
#1820=LINE('',#9322,#2364);
#1821=LINE('',#9325,#2365);
#1822=LINE('',#9326,#2366);
#1823=LINE('',#9329,#2367);
#1824=LINE('',#9330,#2368);
#1825=LINE('',#9333,#2369);
#1826=LINE('',#9334,#2370);
#1827=LINE('',#9337,#2371);
#1828=LINE('',#9338,#2372);
#1829=LINE('',#9341,#2373);
#1830=LINE('',#9342,#2374);
#1831=LINE('',#9345,#2375);
#1832=LINE('',#9346,#2376);
#1833=LINE('',#9349,#2377);
#1834=LINE('',#9350,#2378);
#1835=LINE('',#9353,#2379);
#1836=LINE('',#9354,#2380);
#1837=LINE('',#9357,#2381);
#1838=LINE('',#9358,#2382);
#1839=LINE('',#9361,#2383);
#1840=LINE('',#9362,#2384);
#1841=LINE('',#9365,#2385);
#1842=LINE('',#9366,#2386);
#1843=LINE('',#9369,#2387);
#1844=LINE('',#9370,#2388);
#1845=LINE('',#9373,#2389);
#1846=LINE('',#9374,#2390);
#1847=LINE('',#9377,#2391);
#1848=LINE('',#9378,#2392);
#1849=LINE('',#9381,#2393);
#1850=LINE('',#9382,#2394);
#1851=LINE('',#9385,#2395);
#1852=LINE('',#9386,#2396);
#1853=LINE('',#9389,#2397);
#1854=LINE('',#9391,#2398);
#1855=LINE('',#9392,#2399);
#1856=LINE('',#9395,#2400);
#1857=LINE('',#9396,#2401);
#1858=LINE('',#9399,#2402);
#1859=LINE('',#9400,#2403);
#1860=LINE('',#9403,#2404);
#1861=LINE('',#9404,#2405);
#1862=LINE('',#9407,#2406);
#1863=LINE('',#9408,#2407);
#1864=LINE('',#9411,#2408);
#1865=LINE('',#9412,#2409);
#1866=LINE('',#9415,#2410);
#1867=LINE('',#9416,#2411);
#1868=LINE('',#9419,#2412);
#1869=LINE('',#9420,#2413);
#1870=LINE('',#9423,#2414);
#1871=LINE('',#9424,#2415);
#1872=LINE('',#9427,#2416);
#1873=LINE('',#9428,#2417);
#1874=LINE('',#9431,#2418);
#1875=LINE('',#9432,#2419);
#1876=LINE('',#9435,#2420);
#1877=LINE('',#9436,#2421);
#1878=LINE('',#9439,#2422);
#1879=LINE('',#9440,#2423);
#1880=LINE('',#9443,#2424);
#1881=LINE('',#9444,#2425);
#1882=LINE('',#9447,#2426);
#1883=LINE('',#9448,#2427);
#1884=LINE('',#9451,#2428);
#1885=LINE('',#9452,#2429);
#1886=LINE('',#9455,#2430);
#1887=LINE('',#9456,#2431);
#1888=LINE('',#9459,#2432);
#1889=LINE('',#9460,#2433);
#1890=LINE('',#9464,#2434);
#1891=LINE('',#9467,#2435);
#1892=LINE('',#9468,#2436);
#1893=LINE('',#9471,#2437);
#1894=LINE('',#9472,#2438);
#1895=LINE('',#9474,#2439);
#1896=LINE('',#9476,#2440);
#1897=LINE('',#9482,#2441);
#1898=LINE('',#9484,#2442);
#1899=LINE('',#9486,#2443);
#1900=LINE('',#9487,#2444);
#1901=LINE('',#9490,#2445);
#1902=LINE('',#9492,#2446);
#1903=LINE('',#9493,#2447);
#1904=LINE('',#9496,#2448);
#1905=LINE('',#9498,#2449);
#1906=LINE('',#9499,#2450);
#1907=LINE('',#9502,#2451);
#1908=LINE('',#9504,#2452);
#1909=LINE('',#9505,#2453);
#1910=LINE('',#9508,#2454);
#1911=LINE('',#9510,#2455);
#1912=LINE('',#9511,#2456);
#1913=LINE('',#9513,#2457);
#1914=LINE('',#9514,#2458);
#1915=LINE('',#9524,#2459);
#1916=LINE('',#9533,#2460);
#1917=LINE('',#9537,#2461);
#1918=LINE('',#9541,#2462);
#1919=LINE('',#9548,#2463);
#1920=LINE('',#9550,#2464);
#1921=LINE('',#9558,#2465);
#1922=LINE('',#9562,#2466);
#1923=LINE('',#9566,#2467);
#1924=LINE('',#9573,#2468);
#1925=LINE('',#9577,#2469);
#1926=LINE('',#9581,#2470);
#1927=LINE('',#9586,#2471);
#1928=LINE('',#9588,#2472);
#1929=LINE('',#9590,#2473);
#1930=LINE('',#9591,#2474);
#1931=LINE('',#9594,#2475);
#1932=LINE('',#9596,#2476);
#1933=LINE('',#9597,#2477);
#1934=LINE('',#9600,#2478);
#1935=LINE('',#9602,#2479);
#1936=LINE('',#9603,#2480);
#1937=LINE('',#9606,#2481);
#1938=LINE('',#9608,#2482);
#1939=LINE('',#9609,#2483);
#1940=LINE('',#9612,#2484);
#1941=LINE('',#9614,#2485);
#1942=LINE('',#9615,#2486);
#1943=LINE('',#9617,#2487);
#1944=LINE('',#9618,#2488);
#1945=LINE('',#9625,#2489);
#1946=LINE('',#9627,#2490);
#1947=LINE('',#9629,#2491);
#1948=LINE('',#9630,#2492);
#1949=LINE('',#9633,#2493);
#1950=LINE('',#9635,#2494);
#1951=LINE('',#9636,#2495);
#1952=LINE('',#9639,#2496);
#1953=LINE('',#9641,#2497);
#1954=LINE('',#9642,#2498);
#1955=LINE('',#9647,#2499);
#1956=LINE('',#9649,#2500);
#1957=LINE('',#9651,#2501);
#1958=LINE('',#9653,#2502);
#1959=LINE('',#9655,#2503);
#1960=LINE('',#9657,#2504);
#1961=LINE('',#9658,#2505);
#1962=LINE('',#9661,#2506);
#1963=LINE('',#9662,#2507);
#1964=LINE('',#9665,#2508);
#1965=LINE('',#9666,#2509);
#1966=LINE('',#9669,#2510);
#1967=LINE('',#9671,#2511);
#1968=LINE('',#9673,#2512);
#1969=LINE('',#9675,#2513);
#1970=LINE('',#9676,#2514);
#1971=LINE('',#9678,#2515);
#1972=LINE('',#9681,#2516);
#1973=LINE('',#9684,#2517);
#1974=LINE('',#9688,#2518);
#1975=LINE('',#9695,#2519);
#1976=LINE('',#9697,#2520);
#1977=LINE('',#9699,#2521);
#1978=LINE('',#9706,#2522);
#1979=LINE('',#9710,#2523);
#1980=LINE('',#9717,#2524);
#1981=LINE('',#9724,#2525);
#1982=LINE('',#9726,#2526);
#1983=LINE('',#9728,#2527);
#1984=LINE('',#9729,#2528);
#1985=LINE('',#9732,#2529);
#1986=LINE('',#9734,#2530);
#1987=LINE('',#9735,#2531);
#1988=LINE('',#9738,#2532);
#1989=LINE('',#9740,#2533);
#1990=LINE('',#9741,#2534);
#1991=LINE('',#9744,#2535);
#1992=LINE('',#9746,#2536);
#1993=LINE('',#9747,#2537);
#1994=LINE('',#9750,#2538);
#1995=LINE('',#9752,#2539);
#1996=LINE('',#9753,#2540);
#1997=LINE('',#9755,#2541);
#1998=LINE('',#9756,#2542);
#1999=LINE('',#9768,#2543);
#2000=LINE('',#9772,#2544);
#2001=LINE('',#9776,#2545);
#2002=LINE('',#9783,#2546);
#2003=LINE('',#9785,#2547);
#2004=LINE('',#9791,#2548);
#2005=LINE('',#9795,#2549);
#2006=LINE('',#9802,#2550);
#2007=LINE('',#9812,#2551);
#2008=LINE('',#9816,#2552);
#2009=LINE('',#9820,#2553);
#2010=LINE('',#9827,#2554);
#2011=LINE('',#9831,#2555);
#2012=LINE('',#9835,#2556);
#2013=LINE('',#9840,#2557);
#2014=LINE('',#9842,#2558);
#2015=LINE('',#9844,#2559);
#2016=LINE('',#9845,#2560);
#2017=LINE('',#9848,#2561);
#2018=LINE('',#9850,#2562);
#2019=LINE('',#9851,#2563);
#2020=LINE('',#9854,#2564);
#2021=LINE('',#9856,#2565);
#2022=LINE('',#9857,#2566);
#2023=LINE('',#9860,#2567);
#2024=LINE('',#9862,#2568);
#2025=LINE('',#9863,#2569);
#2026=LINE('',#9866,#2570);
#2027=LINE('',#9868,#2571);
#2028=LINE('',#9869,#2572);
#2029=LINE('',#9871,#2573);
#2030=LINE('',#9872,#2574);
#2031=VECTOR('',#6434,0.274999999999999);
#2032=VECTOR('',#6441,2.);
#2033=VECTOR('',#6454,0.600000000000001);
#2034=VECTOR('',#6461,2.);
#2035=VECTOR('',#6474,0.274999999999999);
#2036=VECTOR('',#6481,2.);
#2037=VECTOR('',#6494,0.600000000000001);
#2038=VECTOR('',#6501,2.);
#2039=VECTOR('',#6514,0.274999999999999);
#2040=VECTOR('',#6521,2.);
#2041=VECTOR('',#6534,0.600000000000001);
#2042=VECTOR('',#6541,2.);
#2043=VECTOR('',#6554,0.274999999999999);
#2044=VECTOR('',#6561,2.);
#2045=VECTOR('',#6574,0.600000000000001);
#2046=VECTOR('',#6581,2.);
#2047=VECTOR('',#6594,0.5);
#2048=VECTOR('',#6605,0.5);
#2049=VECTOR('',#6616,0.5);
#2050=VECTOR('',#6627,0.5);
#2051=VECTOR('',#6638,0.274999999999999);
#2052=VECTOR('',#6643,0.274999999999999);
#2053=VECTOR('',#6648,0.274999999999999);
#2054=VECTOR('',#6653,0.274999999999999);
#2055=VECTOR('',#6656,1.);
#2056=VECTOR('',#6657,1.);
#2057=VECTOR('',#6658,1.);
#2058=VECTOR('',#6659,1.);
#2059=VECTOR('',#6662,1.);
#2060=VECTOR('',#6663,1.);
#2061=VECTOR('',#6664,1.);
#2062=VECTOR('',#6667,1.);
#2063=VECTOR('',#6668,1.);
#2064=VECTOR('',#6669,1.);
#2065=VECTOR('',#6672,1.);
#2066=VECTOR('',#6673,1.);
#2067=VECTOR('',#6684,0.274999999999999);
#2068=VECTOR('',#6691,0.274999999999999);
#2069=VECTOR('',#6698,0.274999999999999);
#2070=VECTOR('',#6705,0.274999999999999);
#2071=VECTOR('',#6710,1.);
#2072=VECTOR('',#6711,1.);
#2073=VECTOR('',#6712,1.);
#2074=VECTOR('',#6713,1.);
#2075=VECTOR('',#6716,1.);
#2076=VECTOR('',#6717,1.);
#2077=VECTOR('',#6718,1.);
#2078=VECTOR('',#6721,1.);
#2079=VECTOR('',#6722,1.);
#2080=VECTOR('',#6723,1.);
#2081=VECTOR('',#6726,1.);
#2082=VECTOR('',#6727,1.);
#2083=VECTOR('',#6728,1.);
#2084=VECTOR('',#6729,1.);
#2085=VECTOR('',#6730,1.);
#2086=VECTOR('',#6731,1.);
#2087=VECTOR('',#6732,1.);
#2088=VECTOR('',#6733,1.);
#2089=VECTOR('',#6734,1.);
#2090=VECTOR('',#6737,1.);
#2091=VECTOR('',#6738,1.);
#2092=VECTOR('',#6739,1.);
#2093=VECTOR('',#6742,1.);
#2094=VECTOR('',#6745,1.);
#2095=VECTOR('',#6746,1.);
#2096=VECTOR('',#6749,1.);
#2097=VECTOR('',#6750,1.);
#2098=VECTOR('',#6751,1.);
#2099=VECTOR('',#6754,1.);
#2100=VECTOR('',#6755,1.);
#2101=VECTOR('',#6758,1.);
#2102=VECTOR('',#6761,1.);
#2103=VECTOR('',#6762,1.);
#2104=VECTOR('',#6765,1.);
#2105=VECTOR('',#6766,1.);
#2106=VECTOR('',#6769,1.);
#2107=VECTOR('',#6778,0.164999999999999);
#2108=VECTOR('',#6785,0.275);
#2109=VECTOR('',#6792,0.275);
#2110=VECTOR('',#6797,1.);
#2111=VECTOR('',#6798,1.);
#2112=VECTOR('',#6799,1.);
#2113=VECTOR('',#6800,1.);
#2114=VECTOR('',#6803,1.);
#2115=VECTOR('',#6804,1.);
#2116=VECTOR('',#6805,1.);
#2117=VECTOR('',#6808,1.);
#2118=VECTOR('',#6809,1.);
#2119=VECTOR('',#6810,1.);
#2120=VECTOR('',#6813,1.);
#2121=VECTOR('',#6814,1.);
#2122=VECTOR('',#6815,1.);
#2123=VECTOR('',#6818,1.);
#2124=VECTOR('',#6819,1.);
#2125=VECTOR('',#6820,1.);
#2126=VECTOR('',#6823,1.);
#2127=VECTOR('',#6824,1.);
#2128=VECTOR('',#6835,0.164999999999999);
#2129=VECTOR('',#6842,0.275);
#2130=VECTOR('',#6849,0.275);
#2131=VECTOR('',#6854,1.);
#2132=VECTOR('',#6855,1.);
#2133=VECTOR('',#6856,1.);
#2134=VECTOR('',#6857,1.);
#2135=VECTOR('',#6860,1.);
#2136=VECTOR('',#6861,1.);
#2137=VECTOR('',#6862,1.);
#2138=VECTOR('',#6865,1.);
#2139=VECTOR('',#6866,1.);
#2140=VECTOR('',#6867,1.);
#2141=VECTOR('',#6870,1.);
#2142=VECTOR('',#6871,1.);
#2143=VECTOR('',#6872,1.);
#2144=VECTOR('',#6875,1.);
#2145=VECTOR('',#6876,1.);
#2146=VECTOR('',#6877,1.);
#2147=VECTOR('',#6880,1.);
#2148=VECTOR('',#6881,1.);
#2149=VECTOR('',#6892,0.225);
#2150=VECTOR('',#6899,0.225);
#2151=VECTOR('',#6904,1.);
#2152=VECTOR('',#6905,1.);
#2153=VECTOR('',#6906,1.);
#2154=VECTOR('',#6907,1.);
#2155=VECTOR('',#6910,1.);
#2156=VECTOR('',#6911,1.);
#2157=VECTOR('',#6912,1.);
#2158=VECTOR('',#6915,1.);
#2159=VECTOR('',#6916,1.);
#2160=VECTOR('',#6917,1.);
#2161=VECTOR('',#6920,1.);
#2162=VECTOR('',#6921,1.);
#2163=VECTOR('',#6932,0.275);
#2164=VECTOR('',#6933,0.275);
#2165=VECTOR('',#6940,0.274999999999999);
#2166=VECTOR('',#6941,0.274999999999999);
#2167=VECTOR('',#6946,0.21);
#2168=VECTOR('',#6949,0.21);
#2169=VECTOR('',#6954,0.275);
#2170=VECTOR('',#6955,0.275);
#2171=VECTOR('',#6962,0.274999999999999);
#2172=VECTOR('',#6963,0.274999999999999);
#2173=VECTOR('',#6968,0.21);
#2174=VECTOR('',#6973,0.21);
#2175=VECTOR('',#6976,1.);
#2176=VECTOR('',#6977,1.);
#2177=VECTOR('',#6978,1.);
#2178=VECTOR('',#6979,1.);
#2179=VECTOR('',#6982,1.);
#2180=VECTOR('',#6983,1.);
#2181=VECTOR('',#6984,1.);
#2182=VECTOR('',#6987,1.);
#2183=VECTOR('',#6988,1.);
#2184=VECTOR('',#6989,1.);
#2185=VECTOR('',#6992,1.);
#2186=VECTOR('',#6993,1.);
#2187=VECTOR('',#6994,1.);
#2188=VECTOR('',#6997,1.);
#2189=VECTOR('',#6998,1.);
#2190=VECTOR('',#6999,1.);
#2191=VECTOR('',#7002,1.);
#2192=VECTOR('',#7003,1.);
#2193=VECTOR('',#7004,1.);
#2194=VECTOR('',#7007,1.);
#2195=VECTOR('',#7008,1.);
#2196=VECTOR('',#7009,1.);
#2197=VECTOR('',#7012,1.);
#2198=VECTOR('',#7013,1.);
#2199=VECTOR('',#7014,1.);
#2200=VECTOR('',#7017,1.);
#2201=VECTOR('',#7018,1.);
#2202=VECTOR('',#7019,1.);
#2203=VECTOR('',#7022,1.);
#2204=VECTOR('',#7023,1.);
#2205=VECTOR('',#7024,1.);
#2206=VECTOR('',#7025,1.);
#2207=VECTOR('',#7028,1.);
#2208=VECTOR('',#7029,1.);
#2209=VECTOR('',#7030,1.);
#2210=VECTOR('',#7033,1.);
#2211=VECTOR('',#7034,1.);
#2212=VECTOR('',#7035,1.);
#2213=VECTOR('',#7038,1.);
#2214=VECTOR('',#7039,1.);
#2215=VECTOR('',#7040,1.);
#2216=VECTOR('',#7043,1.);
#2217=VECTOR('',#7044,1.);
#2218=VECTOR('',#7045,1.);
#2219=VECTOR('',#7048,1.);
#2220=VECTOR('',#7049,1.);
#2221=VECTOR('',#7050,1.);
#2222=VECTOR('',#7053,1.);
#2223=VECTOR('',#7054,1.);
#2224=VECTOR('',#7055,1.);
#2225=VECTOR('',#7058,1.);
#2226=VECTOR('',#7059,1.);
#2227=VECTOR('',#7060,1.);
#2228=VECTOR('',#7063,1.);
#2229=VECTOR('',#7064,1.);
#2230=VECTOR('',#7065,1.);
#2231=VECTOR('',#7068,1.);
#2232=VECTOR('',#7069,1.);
#2233=VECTOR('',#7070,1.);
#2234=VECTOR('',#7071,1.);
#2235=VECTOR('',#7074,1.);
#2236=VECTOR('',#7075,1.);
#2237=VECTOR('',#7076,1.);
#2238=VECTOR('',#7079,1.);
#2239=VECTOR('',#7080,1.);
#2240=VECTOR('',#7081,1.);
#2241=VECTOR('',#7084,1.);
#2242=VECTOR('',#7085,1.);
#2243=VECTOR('',#7086,1.);
#2244=VECTOR('',#7089,1.);
#2245=VECTOR('',#7090,1.);
#2246=VECTOR('',#7091,1.);
#2247=VECTOR('',#7094,1.);
#2248=VECTOR('',#7095,1.);
#2249=VECTOR('',#7096,1.);
#2250=VECTOR('',#7099,1.);
#2251=VECTOR('',#7100,1.);
#2252=VECTOR('',#7101,1.);
#2253=VECTOR('',#7104,1.);
#2254=VECTOR('',#7105,1.);
#2255=VECTOR('',#7106,1.);
#2256=VECTOR('',#7109,1.);
#2257=VECTOR('',#7110,1.);
#2258=VECTOR('',#7111,1.);
#2259=VECTOR('',#7114,1.);
#2260=VECTOR('',#7115,1.);
#2261=VECTOR('',#7116,1.);
#2262=VECTOR('',#7117,1.);
#2263=VECTOR('',#7120,1.);
#2264=VECTOR('',#7121,1.);
#2265=VECTOR('',#7122,1.);
#2266=VECTOR('',#7125,1.);
#2267=VECTOR('',#7126,1.);
#2268=VECTOR('',#7127,1.);
#2269=VECTOR('',#7130,1.);
#2270=VECTOR('',#7131,1.);
#2271=VECTOR('',#7132,1.);
#2272=VECTOR('',#7135,1.);
#2273=VECTOR('',#7136,1.);
#2274=VECTOR('',#7137,1.);
#2275=VECTOR('',#7140,1.);
#2276=VECTOR('',#7141,1.);
#2277=VECTOR('',#7142,1.);
#2278=VECTOR('',#7145,1.);
#2279=VECTOR('',#7146,1.);
#2280=VECTOR('',#7147,1.);
#2281=VECTOR('',#7150,1.);
#2282=VECTOR('',#7151,1.);
#2283=VECTOR('',#7152,1.);
#2284=VECTOR('',#7155,1.);
#2285=VECTOR('',#7156,1.);
#2286=VECTOR('',#7157,1.);
#2287=VECTOR('',#7160,0.21);
#2288=VECTOR('',#7165,1.);
#2289=VECTOR('',#7166,1.);
#2290=VECTOR('',#7167,1.);
#2291=VECTOR('',#7170,1.);
#2292=VECTOR('',#7171,1.);
#2293=VECTOR('',#7172,1.);
#2294=VECTOR('',#7175,1.);
#2295=VECTOR('',#7176,1.);
#2296=VECTOR('',#7179,1.);
#2297=VECTOR('',#7180,1.);
#2298=VECTOR('',#7181,1.);
#2299=VECTOR('',#7184,1.);
#2300=VECTOR('',#7185,1.);
#2301=VECTOR('',#7188,1.);
#2302=VECTOR('',#7189,1.);
#2303=VECTOR('',#7190,1.);
#2304=VECTOR('',#7193,1.);
#2305=VECTOR('',#7194,1.);
#2306=VECTOR('',#7197,1.);
#2307=VECTOR('',#7198,1.);
#2308=VECTOR('',#7207,1.);
#2309=VECTOR('',#7208,1.);
#2310=VECTOR('',#7209,1.);
#2311=VECTOR('',#7210,1.);
#2312=VECTOR('',#7211,1.);
#2313=VECTOR('',#7212,1.);
#2314=VECTOR('',#7213,1.);
#2315=VECTOR('',#7214,1.);
#2316=VECTOR('',#7215,1.);
#2317=VECTOR('',#7216,1.);
#2318=VECTOR('',#7217,1.);
#2319=VECTOR('',#7218,1.);
#2320=VECTOR('',#7219,1.);
#2321=VECTOR('',#7220,1.);
#2322=VECTOR('',#7221,1.);
#2323=VECTOR('',#7222,1.);
#2324=VECTOR('',#7223,1.);
#2325=VECTOR('',#7224,1.);
#2326=VECTOR('',#7225,1.);
#2327=VECTOR('',#7226,1.);
#2328=VECTOR('',#7227,1.);
#2329=VECTOR('',#7228,1.);
#2330=VECTOR('',#7229,1.);
#2331=VECTOR('',#7230,1.);
#2332=VECTOR('',#7231,1.);
#2333=VECTOR('',#7232,1.);
#2334=VECTOR('',#7233,1.);
#2335=VECTOR('',#7234,1.);
#2336=VECTOR('',#7235,1.);
#2337=VECTOR('',#7236,1.);
#2338=VECTOR('',#7237,1.);
#2339=VECTOR('',#7238,1.);
#2340=VECTOR('',#7239,1.);
#2341=VECTOR('',#7240,1.);
#2342=VECTOR('',#7241,1.);
#2343=VECTOR('',#7242,1.);
#2344=VECTOR('',#7243,1.);
#2345=VECTOR('',#7244,1.);
#2346=VECTOR('',#7245,1.);
#2347=VECTOR('',#7246,1.);
#2348=VECTOR('',#7247,1.);
#2349=VECTOR('',#7248,1.);
#2350=VECTOR('',#7249,1.);
#2351=VECTOR('',#7250,1.);
#2352=VECTOR('',#7255,1.);
#2353=VECTOR('',#7256,1.);
#2354=VECTOR('',#7257,1.);
#2355=VECTOR('',#7260,1.);
#2356=VECTOR('',#7261,1.);
#2357=VECTOR('',#7264,1.);
#2358=VECTOR('',#7265,1.);
#2359=VECTOR('',#7268,1.);
#2360=VECTOR('',#7269,1.);
#2361=VECTOR('',#7272,1.);
#2362=VECTOR('',#7273,1.);
#2363=VECTOR('',#7276,1.);
#2364=VECTOR('',#7277,1.);
#2365=VECTOR('',#7280,1.);
#2366=VECTOR('',#7281,1.);
#2367=VECTOR('',#7284,1.);
#2368=VECTOR('',#7285,1.);
#2369=VECTOR('',#7288,1.);
#2370=VECTOR('',#7289,1.);
#2371=VECTOR('',#7292,1.);
#2372=VECTOR('',#7293,1.);
#2373=VECTOR('',#7296,1.);
#2374=VECTOR('',#7297,1.);
#2375=VECTOR('',#7300,1.);
#2376=VECTOR('',#7301,1.);
#2377=VECTOR('',#7304,1.);
#2378=VECTOR('',#7305,1.);
#2379=VECTOR('',#7308,1.);
#2380=VECTOR('',#7309,1.);
#2381=VECTOR('',#7312,1.);
#2382=VECTOR('',#7313,1.);
#2383=VECTOR('',#7316,1.);
#2384=VECTOR('',#7317,1.);
#2385=VECTOR('',#7320,1.);
#2386=VECTOR('',#7321,1.);
#2387=VECTOR('',#7324,1.);
#2388=VECTOR('',#7325,1.);
#2389=VECTOR('',#7328,1.);
#2390=VECTOR('',#7329,1.);
#2391=VECTOR('',#7332,1.);
#2392=VECTOR('',#7333,1.);
#2393=VECTOR('',#7336,1.);
#2394=VECTOR('',#7337,1.);
#2395=VECTOR('',#7340,1.);
#2396=VECTOR('',#7341,1.);
#2397=VECTOR('',#7344,1.);
#2398=VECTOR('',#7345,1.);
#2399=VECTOR('',#7346,1.);
#2400=VECTOR('',#7349,1.);
#2401=VECTOR('',#7350,1.);
#2402=VECTOR('',#7353,1.);
#2403=VECTOR('',#7354,1.);
#2404=VECTOR('',#7357,1.);
#2405=VECTOR('',#7358,1.);
#2406=VECTOR('',#7361,1.);
#2407=VECTOR('',#7362,1.);
#2408=VECTOR('',#7365,1.);
#2409=VECTOR('',#7366,1.);
#2410=VECTOR('',#7369,1.);
#2411=VECTOR('',#7370,1.);
#2412=VECTOR('',#7373,1.);
#2413=VECTOR('',#7374,1.);
#2414=VECTOR('',#7377,1.);
#2415=VECTOR('',#7378,1.);
#2416=VECTOR('',#7381,1.);
#2417=VECTOR('',#7382,1.);
#2418=VECTOR('',#7385,1.);
#2419=VECTOR('',#7386,1.);
#2420=VECTOR('',#7389,1.);
#2421=VECTOR('',#7390,1.);
#2422=VECTOR('',#7393,1.);
#2423=VECTOR('',#7394,1.);
#2424=VECTOR('',#7397,1.);
#2425=VECTOR('',#7398,1.);
#2426=VECTOR('',#7401,1.);
#2427=VECTOR('',#7402,1.);
#2428=VECTOR('',#7405,1.);
#2429=VECTOR('',#7406,1.);
#2430=VECTOR('',#7409,1.);
#2431=VECTOR('',#7410,1.);
#2432=VECTOR('',#7413,1.);
#2433=VECTOR('',#7414,1.);
#2434=VECTOR('',#7419,0.21);
#2435=VECTOR('',#7422,1.);
#2436=VECTOR('',#7423,1.);
#2437=VECTOR('',#7426,1.);
#2438=VECTOR('',#7427,1.);
#2439=VECTOR('',#7430,1.);
#2440=VECTOR('',#7433,1.);
#2441=VECTOR('',#7440,1.);
#2442=VECTOR('',#7441,1.);
#2443=VECTOR('',#7442,1.);
#2444=VECTOR('',#7443,1.);
#2445=VECTOR('',#7446,1.);
#2446=VECTOR('',#7447,1.);
#2447=VECTOR('',#7448,1.);
#2448=VECTOR('',#7451,1.);
#2449=VECTOR('',#7452,1.);
#2450=VECTOR('',#7453,1.);
#2451=VECTOR('',#7456,1.);
#2452=VECTOR('',#7457,1.);
#2453=VECTOR('',#7458,1.);
#2454=VECTOR('',#7461,1.);
#2455=VECTOR('',#7462,1.);
#2456=VECTOR('',#7463,1.);
#2457=VECTOR('',#7466,1.);
#2458=VECTOR('',#7467,1.);
#2459=VECTOR('',#7480,0.25);
#2460=VECTOR('',#7493,0.4);
#2461=VECTOR('',#7498,0.425);
#2462=VECTOR('',#7503,0.41);
#2463=VECTOR('',#7512,0.26);
#2464=VECTOR('',#7515,0.25);
#2465=VECTOR('',#7526,0.4);
#2466=VECTOR('',#7531,0.425);
#2467=VECTOR('',#7536,0.41);
#2468=VECTOR('',#7545,0.26);
#2469=VECTOR('',#7550,0.25);
#2470=VECTOR('',#7555,0.225);
#2471=VECTOR('',#7560,1.);
#2472=VECTOR('',#7561,1.);
#2473=VECTOR('',#7562,1.);
#2474=VECTOR('',#7563,1.);
#2475=VECTOR('',#7566,1.);
#2476=VECTOR('',#7567,1.);
#2477=VECTOR('',#7568,1.);
#2478=VECTOR('',#7571,1.);
#2479=VECTOR('',#7572,1.);
#2480=VECTOR('',#7573,1.);
#2481=VECTOR('',#7576,1.);
#2482=VECTOR('',#7577,1.);
#2483=VECTOR('',#7578,1.);
#2484=VECTOR('',#7581,1.);
#2485=VECTOR('',#7582,1.);
#2486=VECTOR('',#7583,1.);
#2487=VECTOR('',#7586,1.);
#2488=VECTOR('',#7587,1.);
#2489=VECTOR('',#7596,1.);
#2490=VECTOR('',#7597,1.);
#2491=VECTOR('',#7598,1.);
#2492=VECTOR('',#7599,1.);
#2493=VECTOR('',#7602,1.);
#2494=VECTOR('',#7603,1.);
#2495=VECTOR('',#7604,1.);
#2496=VECTOR('',#7607,1.);
#2497=VECTOR('',#7608,1.);
#2498=VECTOR('',#7609,1.);
#2499=VECTOR('',#7614,1.);
#2500=VECTOR('',#7615,1.);
#2501=VECTOR('',#7616,1.);
#2502=VECTOR('',#7617,1.);
#2503=VECTOR('',#7618,1.);
#2504=VECTOR('',#7619,1.);
#2505=VECTOR('',#7620,1.);
#2506=VECTOR('',#7623,1.);
#2507=VECTOR('',#7624,1.);
#2508=VECTOR('',#7627,1.);
#2509=VECTOR('',#7628,1.);
#2510=VECTOR('',#7631,1.);
#2511=VECTOR('',#7632,1.);
#2512=VECTOR('',#7633,1.);
#2513=VECTOR('',#7634,1.);
#2514=VECTOR('',#7635,1.);
#2515=VECTOR('',#7638,1.);
#2516=VECTOR('',#7641,1.);
#2517=VECTOR('',#7644,1.);
#2518=VECTOR('',#7649,0.21);
#2519=VECTOR('',#7658,1.);
#2520=VECTOR('',#7661,1.);
#2521=VECTOR('',#7664,1.);
#2522=VECTOR('',#7673,0.275);
#2523=VECTOR('',#7678,0.265);
#2524=VECTOR('',#7687,0.5);
#2525=VECTOR('',#7696,1.);
#2526=VECTOR('',#7697,1.);
#2527=VECTOR('',#7698,1.);
#2528=VECTOR('',#7699,1.);
#2529=VECTOR('',#7702,1.);
#2530=VECTOR('',#7703,1.);
#2531=VECTOR('',#7704,1.);
#2532=VECTOR('',#7707,1.);
#2533=VECTOR('',#7708,1.);
#2534=VECTOR('',#7709,1.);
#2535=VECTOR('',#7712,1.);
#2536=VECTOR('',#7713,1.);
#2537=VECTOR('',#7714,1.);
#2538=VECTOR('',#7717,1.);
#2539=VECTOR('',#7718,1.);
#2540=VECTOR('',#7719,1.);
#2541=VECTOR('',#7722,1.);
#2542=VECTOR('',#7723,1.);
#2543=VECTOR('',#7740,0.4);
#2544=VECTOR('',#7745,0.425);
#2545=VECTOR('',#7750,0.41);
#2546=VECTOR('',#7759,0.26);
#2547=VECTOR('',#7762,0.25);
#2548=VECTOR('',#7769,0.225);
#2549=VECTOR('',#7774,0.215);
#2550=VECTOR('',#7783,0.45);
#2551=VECTOR('',#7798,0.325);
#2552=VECTOR('',#7803,0.35);
#2553=VECTOR('',#7808,0.335);
#2554=VECTOR('',#7817,0.21);
#2555=VECTOR('',#7822,0.2);
#2556=VECTOR('',#7827,0.18);
#2557=VECTOR('',#7832,1.);
#2558=VECTOR('',#7833,1.);
#2559=VECTOR('',#7834,1.);
#2560=VECTOR('',#7835,1.);
#2561=VECTOR('',#7838,1.);
#2562=VECTOR('',#7839,1.);
#2563=VECTOR('',#7840,1.);
#2564=VECTOR('',#7843,1.);
#2565=VECTOR('',#7844,1.);
#2566=VECTOR('',#7845,1.);
#2567=VECTOR('',#7848,1.);
#2568=VECTOR('',#7849,1.);
#2569=VECTOR('',#7850,1.);
#2570=VECTOR('',#7853,1.);
#2571=VECTOR('',#7854,1.);
#2572=VECTOR('',#7855,1.);
#2573=VECTOR('',#7858,1.);
#2574=VECTOR('',#7859,1.);
#2575=CIRCLE('',#5885,0.274999999999999);
#2576=CIRCLE('',#5886,0.274999999999999);
#2577=CIRCLE('',#5888,2.);
#2578=CIRCLE('',#5889,2.);
#2579=CIRCLE('',#5894,0.600000000000001);
#2580=CIRCLE('',#5895,0.600000000000001);
#2581=CIRCLE('',#5897,2.);
#2582=CIRCLE('',#5898,2.);
#2583=CIRCLE('',#5903,0.274999999999999);
#2584=CIRCLE('',#5904,0.274999999999999);
#2585=CIRCLE('',#5906,2.);
#2586=CIRCLE('',#5907,2.);
#2587=CIRCLE('',#5912,0.600000000000001);
#2588=CIRCLE('',#5913,0.600000000000001);
#2589=CIRCLE('',#5915,2.);
#2590=CIRCLE('',#5916,2.);
#2591=CIRCLE('',#5921,0.274999999999999);
#2592=CIRCLE('',#5922,0.274999999999999);
#2593=CIRCLE('',#5924,2.);
#2594=CIRCLE('',#5925,2.);
#2595=CIRCLE('',#5930,0.600000000000001);
#2596=CIRCLE('',#5931,0.600000000000001);
#2597=CIRCLE('',#5933,2.);
#2598=CIRCLE('',#5934,2.);
#2599=CIRCLE('',#5939,0.274999999999999);
#2600=CIRCLE('',#5940,0.274999999999999);
#2601=CIRCLE('',#5942,2.);
#2602=CIRCLE('',#5943,2.);
#2603=CIRCLE('',#5948,0.600000000000001);
#2604=CIRCLE('',#5949,0.600000000000001);
#2605=CIRCLE('',#5951,2.);
#2606=CIRCLE('',#5952,2.);
#2607=CIRCLE('',#5957,0.5);
#2608=CIRCLE('',#5958,0.5);
#2609=CIRCLE('',#5960,0.274999999999999);
#2610=CIRCLE('',#5962,0.5);
#2611=CIRCLE('',#5963,0.5);
#2612=CIRCLE('',#5965,0.274999999999999);
#2613=CIRCLE('',#5967,0.5);
#2614=CIRCLE('',#5968,0.5);
#2615=CIRCLE('',#5970,0.274999999999999);
#2616=CIRCLE('',#5972,0.5);
#2617=CIRCLE('',#5973,0.5);
#2618=CIRCLE('',#5975,0.274999999999999);
#2619=CIRCLE('',#5977,0.274999999999999);
#2620=CIRCLE('',#5979,0.274999999999999);
#2621=CIRCLE('',#5981,0.274999999999999);
#2622=CIRCLE('',#5983,0.274999999999999);
#2623=CIRCLE('',#5992,0.274999999999999);
#2624=CIRCLE('',#5993,0.274999999999999);
#2625=CIRCLE('',#5995,0.274999999999999);
#2626=CIRCLE('',#5996,0.274999999999999);
#2627=CIRCLE('',#5998,0.274999999999999);
#2628=CIRCLE('',#5999,0.274999999999999);
#2629=CIRCLE('',#6001,0.274999999999999);
#2630=CIRCLE('',#6002,0.274999999999999);
#2631=CIRCLE('',#6019,0.164999999999999);
#2632=CIRCLE('',#6020,0.164999999999999);
#2633=CIRCLE('',#6022,0.275);
#2634=CIRCLE('',#6023,0.275);
#2635=CIRCLE('',#6025,0.275);
#2636=CIRCLE('',#6026,0.275);
#2637=CIRCLE('',#6037,0.164999999999999);
#2638=CIRCLE('',#6038,0.164999999999999);
#2639=CIRCLE('',#6040,0.275);
#2640=CIRCLE('',#6041,0.275);
#2641=CIRCLE('',#6043,0.275);
#2642=CIRCLE('',#6044,0.275);
#2643=CIRCLE('',#6055,0.225);
#2644=CIRCLE('',#6056,0.225);
#2645=CIRCLE('',#6058,0.225);
#2646=CIRCLE('',#6059,0.225);
#2647=CIRCLE('',#6068,0.275);
#2648=CIRCLE('',#6069,0.275);
#2649=CIRCLE('',#6071,0.274999999999999);
#2650=CIRCLE('',#6072,0.274999999999999);
#2651=CIRCLE('',#6076,0.275);
#2652=CIRCLE('',#6077,0.275);
#2653=CIRCLE('',#6079,0.274999999999999);
#2654=CIRCLE('',#6080,0.274999999999999);
#2655=CIRCLE('',#6083,0.21);
#2656=CIRCLE('',#6121,0.21);
#2657=CIRCLE('',#6134,0.21);
#2658=CIRCLE('',#6176,0.21);
#2659=CIRCLE('',#6192,0.25);
#2660=CIRCLE('',#6193,0.24505);
#2661=CIRCLE('',#6195,0.25);
#2662=CIRCLE('',#6198,0.375);
#2663=CIRCLE('',#6200,0.425);
#2664=CIRCLE('',#6202,0.425);
#2665=CIRCLE('',#6204,0.395);
#2666=CIRCLE('',#6206,0.27);
#2667=CIRCLE('',#6208,0.24505);
#2668=CIRCLE('',#6212,0.375);
#2669=CIRCLE('',#6214,0.425);
#2670=CIRCLE('',#6216,0.425);
#2671=CIRCLE('',#6218,0.395);
#2672=CIRCLE('',#6220,0.27);
#2673=CIRCLE('',#6222,0.24505);
#2674=CIRCLE('',#6224,0.24505);
#2675=CIRCLE('',#6226,0.2);
#2676=CIRCLE('',#6240,0.2117);
#2677=CIRCLE('',#6249,0.2117);
#2678=CIRCLE('',#6250,0.2117);
#2679=CIRCLE('',#6252,0.2117);
#2680=CIRCLE('',#6259,0.285);
#2681=CIRCLE('',#6260,0.265);
#2682=CIRCLE('',#6262,0.265);
#2683=CIRCLE('',#6264,0.5);
#2684=CIRCLE('',#6266,0.5);
#2685=CIRCLE('',#6278,0.24505);
#2686=CIRCLE('',#6280,0.375);
#2687=CIRCLE('',#6282,0.425);
#2688=CIRCLE('',#6284,0.425);
#2689=CIRCLE('',#6286,0.395);
#2690=CIRCLE('',#6288,0.27);
#2691=CIRCLE('',#6290,0.24505);
#2692=CIRCLE('',#6294,0.235);
#2693=CIRCLE('',#6295,0.215);
#2694=CIRCLE('',#6297,0.215);
#2695=CIRCLE('',#6299,0.45);
#2696=CIRCLE('',#6301,0.45);
#2697=CIRCLE('',#6305,0.3);
#2698=CIRCLE('',#6307,0.35);
#2699=CIRCLE('',#6309,0.35);
#2700=CIRCLE('',#6311,0.32);
#2701=CIRCLE('',#6313,0.22);
#2702=CIRCLE('',#6315,0.1954);
#2703=CIRCLE('',#6317,0.1954);
#2704=CIRCLE('',#6319,0.16);
#2705=VERTEX_POINT('',#8061);
#2706=VERTEX_POINT('',#8063);
#2707=VERTEX_POINT('',#8067);
#2708=VERTEX_POINT('',#8069);
#2709=VERTEX_POINT('',#8076);
#2710=VERTEX_POINT('',#8078);
#2711=VERTEX_POINT('',#8082);
#2712=VERTEX_POINT('',#8084);
#2713=VERTEX_POINT('',#8091);
#2714=VERTEX_POINT('',#8093);
#2715=VERTEX_POINT('',#8097);
#2716=VERTEX_POINT('',#8099);
#2717=VERTEX_POINT('',#8106);
#2718=VERTEX_POINT('',#8108);
#2719=VERTEX_POINT('',#8112);
#2720=VERTEX_POINT('',#8114);
#2721=VERTEX_POINT('',#8121);
#2722=VERTEX_POINT('',#8123);
#2723=VERTEX_POINT('',#8127);
#2724=VERTEX_POINT('',#8129);
#2725=VERTEX_POINT('',#8136);
#2726=VERTEX_POINT('',#8138);
#2727=VERTEX_POINT('',#8142);
#2728=VERTEX_POINT('',#8144);
#2729=VERTEX_POINT('',#8151);
#2730=VERTEX_POINT('',#8153);
#2731=VERTEX_POINT('',#8157);
#2732=VERTEX_POINT('',#8159);
#2733=VERTEX_POINT('',#8166);
#2734=VERTEX_POINT('',#8168);
#2735=VERTEX_POINT('',#8172);
#2736=VERTEX_POINT('',#8174);
#2737=VERTEX_POINT('',#8181);
#2738=VERTEX_POINT('',#8183);
#2739=VERTEX_POINT('',#8187);
#2740=VERTEX_POINT('',#8190);
#2741=VERTEX_POINT('',#8192);
#2742=VERTEX_POINT('',#8196);
#2743=VERTEX_POINT('',#8199);
#2744=VERTEX_POINT('',#8201);
#2745=VERTEX_POINT('',#8205);
#2746=VERTEX_POINT('',#8208);
#2747=VERTEX_POINT('',#8210);
#2748=VERTEX_POINT('',#8214);
#2749=VERTEX_POINT('',#8217);
#2750=VERTEX_POINT('',#8221);
#2751=VERTEX_POINT('',#8225);
#2752=VERTEX_POINT('',#8229);
#2753=VERTEX_POINT('',#8233);
#2754=VERTEX_POINT('',#8234);
#2755=VERTEX_POINT('',#8236);
#2756=VERTEX_POINT('',#8238);
#2757=VERTEX_POINT('',#8242);
#2758=VERTEX_POINT('',#8244);
#2759=VERTEX_POINT('',#8248);
#2760=VERTEX_POINT('',#8250);
#2761=VERTEX_POINT('',#8260);
#2762=VERTEX_POINT('',#8262);
#2763=VERTEX_POINT('',#8266);
#2764=VERTEX_POINT('',#8268);
#2765=VERTEX_POINT('',#8272);
#2766=VERTEX_POINT('',#8274);
#2767=VERTEX_POINT('',#8278);
#2768=VERTEX_POINT('',#8280);
#2769=VERTEX_POINT('',#8284);
#2770=VERTEX_POINT('',#8285);
#2771=VERTEX_POINT('',#8287);
#2772=VERTEX_POINT('',#8289);
#2773=VERTEX_POINT('',#8293);
#2774=VERTEX_POINT('',#8295);
#2775=VERTEX_POINT('',#8299);
#2776=VERTEX_POINT('',#8301);
#2777=VERTEX_POINT('',#8305);
#2778=VERTEX_POINT('',#8307);
#2779=VERTEX_POINT('',#8309);
#2780=VERTEX_POINT('',#8311);
#2781=VERTEX_POINT('',#8313);
#2782=VERTEX_POINT('',#8315);
#2783=VERTEX_POINT('',#8317);
#2784=VERTEX_POINT('',#8319);
#2785=VERTEX_POINT('',#8323);
#2786=VERTEX_POINT('',#8324);
#2787=VERTEX_POINT('',#8331);
#2788=VERTEX_POINT('',#8335);
#2789=VERTEX_POINT('',#8336);
#2790=VERTEX_POINT('',#8341);
#2791=VERTEX_POINT('',#8347);
#2792=VERTEX_POINT('',#8351);
#2793=VERTEX_POINT('',#8359);
#2794=VERTEX_POINT('',#8361);
#2795=VERTEX_POINT('',#8365);
#2796=VERTEX_POINT('',#8367);
#2797=VERTEX_POINT('',#8371);
#2798=VERTEX_POINT('',#8373);
#2799=VERTEX_POINT('',#8377);
#2800=VERTEX_POINT('',#8378);
#2801=VERTEX_POINT('',#8380);
#2802=VERTEX_POINT('',#8382);
#2803=VERTEX_POINT('',#8386);
#2804=VERTEX_POINT('',#8388);
#2805=VERTEX_POINT('',#8392);
#2806=VERTEX_POINT('',#8394);
#2807=VERTEX_POINT('',#8398);
#2808=VERTEX_POINT('',#8400);
#2809=VERTEX_POINT('',#8404);
#2810=VERTEX_POINT('',#8406);
#2811=VERTEX_POINT('',#8416);
#2812=VERTEX_POINT('',#8418);
#2813=VERTEX_POINT('',#8422);
#2814=VERTEX_POINT('',#8424);
#2815=VERTEX_POINT('',#8428);
#2816=VERTEX_POINT('',#8430);
#2817=VERTEX_POINT('',#8434);
#2818=VERTEX_POINT('',#8435);
#2819=VERTEX_POINT('',#8437);
#2820=VERTEX_POINT('',#8439);
#2821=VERTEX_POINT('',#8443);
#2822=VERTEX_POINT('',#8445);
#2823=VERTEX_POINT('',#8449);
#2824=VERTEX_POINT('',#8451);
#2825=VERTEX_POINT('',#8455);
#2826=VERTEX_POINT('',#8457);
#2827=VERTEX_POINT('',#8461);
#2828=VERTEX_POINT('',#8463);
#2829=VERTEX_POINT('',#8473);
#2830=VERTEX_POINT('',#8475);
#2831=VERTEX_POINT('',#8479);
#2832=VERTEX_POINT('',#8481);
#2833=VERTEX_POINT('',#8485);
#2834=VERTEX_POINT('',#8486);
#2835=VERTEX_POINT('',#8488);
#2836=VERTEX_POINT('',#8490);
#2837=VERTEX_POINT('',#8494);
#2838=VERTEX_POINT('',#8496);
#2839=VERTEX_POINT('',#8500);
#2840=VERTEX_POINT('',#8502);
#2841=VERTEX_POINT('',#8512);
#2842=VERTEX_POINT('',#8514);
#2843=VERTEX_POINT('',#8516);
#2844=VERTEX_POINT('',#8529);
#2845=VERTEX_POINT('',#8542);
#2846=VERTEX_POINT('',#8545);
#2847=VERTEX_POINT('',#8570);
#2848=VERTEX_POINT('',#8571);
#2849=VERTEX_POINT('',#8617);
#2850=VERTEX_POINT('',#8619);
#2851=VERTEX_POINT('',#8621);
#2852=VERTEX_POINT('',#8634);
#2853=VERTEX_POINT('',#8647);
#2854=VERTEX_POINT('',#8650);
#2855=VERTEX_POINT('',#8675);
#2856=VERTEX_POINT('',#8676);
#2857=VERTEX_POINT('',#8724);
#2858=VERTEX_POINT('',#8725);
#2859=VERTEX_POINT('',#8772);
#2860=VERTEX_POINT('',#8774);
#2861=VERTEX_POINT('',#8776);
#2862=VERTEX_POINT('',#8799);
#2863=VERTEX_POINT('',#8802);
#2864=VERTEX_POINT('',#8828);
#2865=VERTEX_POINT('',#8830);
#2866=VERTEX_POINT('',#8832);
#2867=VERTEX_POINT('',#8855);
#2868=VERTEX_POINT('',#8858);
#2869=VERTEX_POINT('',#8883);
#2870=VERTEX_POINT('',#8884);
#2871=VERTEX_POINT('',#8932);
#2872=VERTEX_POINT('',#8936);
#2873=VERTEX_POINT('',#8937);
#2874=VERTEX_POINT('',#8939);
#2875=VERTEX_POINT('',#8941);
#2876=VERTEX_POINT('',#8945);
#2877=VERTEX_POINT('',#8947);
#2878=VERTEX_POINT('',#8951);
#2879=VERTEX_POINT('',#8953);
#2880=VERTEX_POINT('',#8957);
#2881=VERTEX_POINT('',#8959);
#2882=VERTEX_POINT('',#8963);
#2883=VERTEX_POINT('',#8965);
#2884=VERTEX_POINT('',#8969);
#2885=VERTEX_POINT('',#8971);
#2886=VERTEX_POINT('',#8975);
#2887=VERTEX_POINT('',#8977);
#2888=VERTEX_POINT('',#8981);
#2889=VERTEX_POINT('',#8983);
#2890=VERTEX_POINT('',#8987);
#2891=VERTEX_POINT('',#8989);
#2892=VERTEX_POINT('',#8993);
#2893=VERTEX_POINT('',#8994);
#2894=VERTEX_POINT('',#8996);
#2895=VERTEX_POINT('',#8998);
#2896=VERTEX_POINT('',#9002);
#2897=VERTEX_POINT('',#9004);
#2898=VERTEX_POINT('',#9008);
#2899=VERTEX_POINT('',#9010);
#2900=VERTEX_POINT('',#9014);
#2901=VERTEX_POINT('',#9016);
#2902=VERTEX_POINT('',#9020);
#2903=VERTEX_POINT('',#9022);
#2904=VERTEX_POINT('',#9026);
#2905=VERTEX_POINT('',#9028);
#2906=VERTEX_POINT('',#9032);
#2907=VERTEX_POINT('',#9034);
#2908=VERTEX_POINT('',#9038);
#2909=VERTEX_POINT('',#9040);
#2910=VERTEX_POINT('',#9044);
#2911=VERTEX_POINT('',#9046);
#2912=VERTEX_POINT('',#9050);
#2913=VERTEX_POINT('',#9051);
#2914=VERTEX_POINT('',#9053);
#2915=VERTEX_POINT('',#9055);
#2916=VERTEX_POINT('',#9059);
#2917=VERTEX_POINT('',#9061);
#2918=VERTEX_POINT('',#9065);
#2919=VERTEX_POINT('',#9067);
#2920=VERTEX_POINT('',#9071);
#2921=VERTEX_POINT('',#9073);
#2922=VERTEX_POINT('',#9077);
#2923=VERTEX_POINT('',#9079);
#2924=VERTEX_POINT('',#9083);
#2925=VERTEX_POINT('',#9085);
#2926=VERTEX_POINT('',#9089);
#2927=VERTEX_POINT('',#9091);
#2928=VERTEX_POINT('',#9095);
#2929=VERTEX_POINT('',#9097);
#2930=VERTEX_POINT('',#9101);
#2931=VERTEX_POINT('',#9103);
#2932=VERTEX_POINT('',#9107);
#2933=VERTEX_POINT('',#9108);
#2934=VERTEX_POINT('',#9110);
#2935=VERTEX_POINT('',#9112);
#2936=VERTEX_POINT('',#9116);
#2937=VERTEX_POINT('',#9118);
#2938=VERTEX_POINT('',#9122);
#2939=VERTEX_POINT('',#9124);
#2940=VERTEX_POINT('',#9128);
#2941=VERTEX_POINT('',#9130);
#2942=VERTEX_POINT('',#9134);
#2943=VERTEX_POINT('',#9136);
#2944=VERTEX_POINT('',#9140);
#2945=VERTEX_POINT('',#9142);
#2946=VERTEX_POINT('',#9146);
#2947=VERTEX_POINT('',#9148);
#2948=VERTEX_POINT('',#9152);
#2949=VERTEX_POINT('',#9154);
#2950=VERTEX_POINT('',#9158);
#2951=VERTEX_POINT('',#9160);
#2952=VERTEX_POINT('',#9164);
#2953=VERTEX_POINT('',#9168);
#2954=VERTEX_POINT('',#9170);
#2955=VERTEX_POINT('',#9174);
#2956=VERTEX_POINT('',#9176);
#2957=VERTEX_POINT('',#9183);
#2958=VERTEX_POINT('',#9185);
#2959=VERTEX_POINT('',#9192);
#2960=VERTEX_POINT('',#9194);
#2961=VERTEX_POINT('',#9207);
#2962=VERTEX_POINT('',#9208);
#2963=VERTEX_POINT('',#9210);
#2964=VERTEX_POINT('',#9212);
#2965=VERTEX_POINT('',#9214);
#2966=VERTEX_POINT('',#9216);
#2967=VERTEX_POINT('',#9218);
#2968=VERTEX_POINT('',#9220);
#2969=VERTEX_POINT('',#9222);
#2970=VERTEX_POINT('',#9224);
#2971=VERTEX_POINT('',#9226);
#2972=VERTEX_POINT('',#9228);
#2973=VERTEX_POINT('',#9230);
#2974=VERTEX_POINT('',#9232);
#2975=VERTEX_POINT('',#9234);
#2976=VERTEX_POINT('',#9236);
#2977=VERTEX_POINT('',#9238);
#2978=VERTEX_POINT('',#9240);
#2979=VERTEX_POINT('',#9242);
#2980=VERTEX_POINT('',#9244);
#2981=VERTEX_POINT('',#9246);
#2982=VERTEX_POINT('',#9248);
#2983=VERTEX_POINT('',#9250);
#2984=VERTEX_POINT('',#9252);
#2985=VERTEX_POINT('',#9254);
#2986=VERTEX_POINT('',#9256);
#2987=VERTEX_POINT('',#9258);
#2988=VERTEX_POINT('',#9260);
#2989=VERTEX_POINT('',#9262);
#2990=VERTEX_POINT('',#9264);
#2991=VERTEX_POINT('',#9266);
#2992=VERTEX_POINT('',#9268);
#2993=VERTEX_POINT('',#9270);
#2994=VERTEX_POINT('',#9272);
#2995=VERTEX_POINT('',#9274);
#2996=VERTEX_POINT('',#9276);
#2997=VERTEX_POINT('',#9278);
#2998=VERTEX_POINT('',#9280);
#2999=VERTEX_POINT('',#9282);
#3000=VERTEX_POINT('',#9284);
#3001=VERTEX_POINT('',#9286);
#3002=VERTEX_POINT('',#9288);
#3003=VERTEX_POINT('',#9290);
#3004=VERTEX_POINT('',#9292);
#3005=VERTEX_POINT('',#9295);
#3006=VERTEX_POINT('',#9298);
#3007=VERTEX_POINT('',#9300);
#3008=VERTEX_POINT('',#9304);
#3009=VERTEX_POINT('',#9308);
#3010=VERTEX_POINT('',#9312);
#3011=VERTEX_POINT('',#9316);
#3012=VERTEX_POINT('',#9320);
#3013=VERTEX_POINT('',#9324);
#3014=VERTEX_POINT('',#9328);
#3015=VERTEX_POINT('',#9332);
#3016=VERTEX_POINT('',#9336);
#3017=VERTEX_POINT('',#9340);
#3018=VERTEX_POINT('',#9344);
#3019=VERTEX_POINT('',#9348);
#3020=VERTEX_POINT('',#9352);
#3021=VERTEX_POINT('',#9356);
#3022=VERTEX_POINT('',#9360);
#3023=VERTEX_POINT('',#9364);
#3024=VERTEX_POINT('',#9368);
#3025=VERTEX_POINT('',#9372);
#3026=VERTEX_POINT('',#9376);
#3027=VERTEX_POINT('',#9380);
#3028=VERTEX_POINT('',#9384);
#3029=VERTEX_POINT('',#9388);
#3030=VERTEX_POINT('',#9390);
#3031=VERTEX_POINT('',#9394);
#3032=VERTEX_POINT('',#9398);
#3033=VERTEX_POINT('',#9402);
#3034=VERTEX_POINT('',#9406);
#3035=VERTEX_POINT('',#9410);
#3036=VERTEX_POINT('',#9414);
#3037=VERTEX_POINT('',#9418);
#3038=VERTEX_POINT('',#9422);
#3039=VERTEX_POINT('',#9426);
#3040=VERTEX_POINT('',#9430);
#3041=VERTEX_POINT('',#9434);
#3042=VERTEX_POINT('',#9438);
#3043=VERTEX_POINT('',#9442);
#3044=VERTEX_POINT('',#9446);
#3045=VERTEX_POINT('',#9450);
#3046=VERTEX_POINT('',#9454);
#3047=VERTEX_POINT('',#9458);
#3048=VERTEX_POINT('',#9462);
#3049=VERTEX_POINT('',#9466);
#3050=VERTEX_POINT('',#9470);
#3051=VERTEX_POINT('',#9480);
#3052=VERTEX_POINT('',#9481);
#3053=VERTEX_POINT('',#9483);
#3054=VERTEX_POINT('',#9485);
#3055=VERTEX_POINT('',#9489);
#3056=VERTEX_POINT('',#9491);
#3057=VERTEX_POINT('',#9495);
#3058=VERTEX_POINT('',#9497);
#3059=VERTEX_POINT('',#9501);
#3060=VERTEX_POINT('',#9503);
#3061=VERTEX_POINT('',#9507);
#3062=VERTEX_POINT('',#9509);
#3063=VERTEX_POINT('',#9518);
#3064=VERTEX_POINT('',#9520);
#3065=VERTEX_POINT('',#9523);
#3066=VERTEX_POINT('',#9528);
#3067=VERTEX_POINT('',#9531);
#3068=VERTEX_POINT('',#9535);
#3069=VERTEX_POINT('',#9539);
#3070=VERTEX_POINT('',#9543);
#3071=VERTEX_POINT('',#9546);
#3072=VERTEX_POINT('',#9553);
#3073=VERTEX_POINT('',#9556);
#3074=VERTEX_POINT('',#9560);
#3075=VERTEX_POINT('',#9564);
#3076=VERTEX_POINT('',#9568);
#3077=VERTEX_POINT('',#9571);
#3078=VERTEX_POINT('',#9575);
#3079=VERTEX_POINT('',#9579);
#3080=VERTEX_POINT('',#9584);
#3081=VERTEX_POINT('',#9585);
#3082=VERTEX_POINT('',#9587);
#3083=VERTEX_POINT('',#9589);
#3084=VERTEX_POINT('',#9593);
#3085=VERTEX_POINT('',#9595);
#3086=VERTEX_POINT('',#9599);
#3087=VERTEX_POINT('',#9601);
#3088=VERTEX_POINT('',#9605);
#3089=VERTEX_POINT('',#9607);
#3090=VERTEX_POINT('',#9611);
#3091=VERTEX_POINT('',#9613);
#3092=VERTEX_POINT('',#9623);
#3093=VERTEX_POINT('',#9624);
#3094=VERTEX_POINT('',#9626);
#3095=VERTEX_POINT('',#9628);
#3096=VERTEX_POINT('',#9632);
#3097=VERTEX_POINT('',#9634);
#3098=VERTEX_POINT('',#9638);
#3099=VERTEX_POINT('',#9640);
#3100=VERTEX_POINT('',#9643);
#3101=VERTEX_POINT('',#9646);
#3102=VERTEX_POINT('',#9648);
#3103=VERTEX_POINT('',#9650);
#3104=VERTEX_POINT('',#9652);
#3105=VERTEX_POINT('',#9654);
#3106=VERTEX_POINT('',#9656);
#3107=VERTEX_POINT('',#9660);
#3108=VERTEX_POINT('',#9664);
#3109=VERTEX_POINT('',#9668);
#3110=VERTEX_POINT('',#9670);
#3111=VERTEX_POINT('',#9672);
#3112=VERTEX_POINT('',#9674);
#3113=VERTEX_POINT('',#9680);
#3114=VERTEX_POINT('',#9682);
#3115=VERTEX_POINT('',#9686);
#3116=VERTEX_POINT('',#9689);
#3117=VERTEX_POINT('',#9691);
#3118=VERTEX_POINT('',#9703);
#3119=VERTEX_POINT('',#9705);
#3120=VERTEX_POINT('',#9709);
#3121=VERTEX_POINT('',#9713);
#3122=VERTEX_POINT('',#9716);
#3123=VERTEX_POINT('',#9722);
#3124=VERTEX_POINT('',#9723);
#3125=VERTEX_POINT('',#9725);
#3126=VERTEX_POINT('',#9727);
#3127=VERTEX_POINT('',#9731);
#3128=VERTEX_POINT('',#9733);
#3129=VERTEX_POINT('',#9737);
#3130=VERTEX_POINT('',#9739);
#3131=VERTEX_POINT('',#9743);
#3132=VERTEX_POINT('',#9745);
#3133=VERTEX_POINT('',#9749);
#3134=VERTEX_POINT('',#9751);
#3135=VERTEX_POINT('',#9760);
#3136=VERTEX_POINT('',#9763);
#3137=VERTEX_POINT('',#9766);
#3138=VERTEX_POINT('',#9770);
#3139=VERTEX_POINT('',#9774);
#3140=VERTEX_POINT('',#9778);
#3141=VERTEX_POINT('',#9781);
#3142=VERTEX_POINT('',#9788);
#3143=VERTEX_POINT('',#9790);
#3144=VERTEX_POINT('',#9794);
#3145=VERTEX_POINT('',#9798);
#3146=VERTEX_POINT('',#9801);
#3147=VERTEX_POINT('',#9807);
#3148=VERTEX_POINT('',#9810);
#3149=VERTEX_POINT('',#9814);
#3150=VERTEX_POINT('',#9818);
#3151=VERTEX_POINT('',#9822);
#3152=VERTEX_POINT('',#9825);
#3153=VERTEX_POINT('',#9829);
#3154=VERTEX_POINT('',#9833);
#3155=VERTEX_POINT('',#9838);
#3156=VERTEX_POINT('',#9839);
#3157=VERTEX_POINT('',#9841);
#3158=VERTEX_POINT('',#9843);
#3159=VERTEX_POINT('',#9847);
#3160=VERTEX_POINT('',#9849);
#3161=VERTEX_POINT('',#9853);
#3162=VERTEX_POINT('',#9855);
#3163=VERTEX_POINT('',#9859);
#3164=VERTEX_POINT('',#9861);
#3165=VERTEX_POINT('',#9865);
#3166=VERTEX_POINT('',#9867);
#3167=EDGE_CURVE('',#2705,#2705,#2575,.T.);
#3168=EDGE_CURVE('',#2705,#2706,#1487,.T.);
#3169=EDGE_CURVE('',#2706,#2706,#2576,.T.);
#3170=EDGE_CURVE('',#2707,#2707,#2577,.T.);
#3171=EDGE_CURVE('',#2707,#2708,#1488,.T.);
#3172=EDGE_CURVE('',#2708,#2708,#2578,.T.);
#3173=EDGE_CURVE('',#2709,#2709,#2579,.T.);
#3174=EDGE_CURVE('',#2709,#2710,#1489,.T.);
#3175=EDGE_CURVE('',#2710,#2710,#2580,.T.);
#3176=EDGE_CURVE('',#2711,#2711,#2581,.T.);
#3177=EDGE_CURVE('',#2711,#2712,#1490,.T.);
#3178=EDGE_CURVE('',#2712,#2712,#2582,.T.);
#3179=EDGE_CURVE('',#2713,#2713,#2583,.T.);
#3180=EDGE_CURVE('',#2713,#2714,#1491,.T.);
#3181=EDGE_CURVE('',#2714,#2714,#2584,.T.);
#3182=EDGE_CURVE('',#2715,#2715,#2585,.T.);
#3183=EDGE_CURVE('',#2715,#2716,#1492,.T.);
#3184=EDGE_CURVE('',#2716,#2716,#2586,.T.);
#3185=EDGE_CURVE('',#2717,#2717,#2587,.T.);
#3186=EDGE_CURVE('',#2717,#2718,#1493,.T.);
#3187=EDGE_CURVE('',#2718,#2718,#2588,.T.);
#3188=EDGE_CURVE('',#2719,#2719,#2589,.T.);
#3189=EDGE_CURVE('',#2719,#2720,#1494,.T.);
#3190=EDGE_CURVE('',#2720,#2720,#2590,.T.);
#3191=EDGE_CURVE('',#2721,#2721,#2591,.T.);
#3192=EDGE_CURVE('',#2721,#2722,#1495,.T.);
#3193=EDGE_CURVE('',#2722,#2722,#2592,.T.);
#3194=EDGE_CURVE('',#2723,#2723,#2593,.T.);
#3195=EDGE_CURVE('',#2723,#2724,#1496,.T.);
#3196=EDGE_CURVE('',#2724,#2724,#2594,.T.);
#3197=EDGE_CURVE('',#2725,#2725,#2595,.T.);
#3198=EDGE_CURVE('',#2725,#2726,#1497,.T.);
#3199=EDGE_CURVE('',#2726,#2726,#2596,.T.);
#3200=EDGE_CURVE('',#2727,#2727,#2597,.T.);
#3201=EDGE_CURVE('',#2727,#2728,#1498,.T.);
#3202=EDGE_CURVE('',#2728,#2728,#2598,.T.);
#3203=EDGE_CURVE('',#2729,#2729,#2599,.T.);
#3204=EDGE_CURVE('',#2729,#2730,#1499,.T.);
#3205=EDGE_CURVE('',#2730,#2730,#2600,.T.);
#3206=EDGE_CURVE('',#2731,#2731,#2601,.T.);
#3207=EDGE_CURVE('',#2731,#2732,#1500,.T.);
#3208=EDGE_CURVE('',#2732,#2732,#2602,.T.);
#3209=EDGE_CURVE('',#2733,#2733,#2603,.T.);
#3210=EDGE_CURVE('',#2733,#2734,#1501,.T.);
#3211=EDGE_CURVE('',#2734,#2734,#2604,.T.);
#3212=EDGE_CURVE('',#2735,#2735,#2605,.T.);
#3213=EDGE_CURVE('',#2735,#2736,#1502,.T.);
#3214=EDGE_CURVE('',#2736,#2736,#2606,.T.);
#3215=EDGE_CURVE('',#2737,#2737,#2607,.T.);
#3216=EDGE_CURVE('',#2737,#2738,#1503,.T.);
#3217=EDGE_CURVE('',#2738,#2738,#2608,.T.);
#3218=EDGE_CURVE('',#2739,#2739,#2609,.T.);
#3219=EDGE_CURVE('',#2740,#2740,#2610,.T.);
#3220=EDGE_CURVE('',#2740,#2741,#1504,.T.);
#3221=EDGE_CURVE('',#2741,#2741,#2611,.T.);
#3222=EDGE_CURVE('',#2742,#2742,#2612,.T.);
#3223=EDGE_CURVE('',#2743,#2743,#2613,.T.);
#3224=EDGE_CURVE('',#2743,#2744,#1505,.T.);
#3225=EDGE_CURVE('',#2744,#2744,#2614,.T.);
#3226=EDGE_CURVE('',#2745,#2745,#2615,.T.);
#3227=EDGE_CURVE('',#2746,#2746,#2616,.T.);
#3228=EDGE_CURVE('',#2746,#2747,#1506,.T.);
#3229=EDGE_CURVE('',#2747,#2747,#2617,.T.);
#3230=EDGE_CURVE('',#2748,#2748,#2618,.T.);
#3231=EDGE_CURVE('',#2749,#2749,#2619,.T.);
#3232=EDGE_CURVE('',#2749,#2739,#1507,.T.);
#3233=EDGE_CURVE('',#2750,#2750,#2620,.T.);
#3234=EDGE_CURVE('',#2750,#2742,#1508,.T.);
#3235=EDGE_CURVE('',#2751,#2751,#2621,.T.);
#3236=EDGE_CURVE('',#2751,#2745,#1509,.T.);
#3237=EDGE_CURVE('',#2752,#2752,#2622,.T.);
#3238=EDGE_CURVE('',#2752,#2748,#1510,.T.);
#3239=EDGE_CURVE('',#2753,#2754,#1511,.T.);
#3240=EDGE_CURVE('',#2754,#2755,#1512,.T.);
#3241=EDGE_CURVE('',#2756,#2755,#1513,.T.);
#3242=EDGE_CURVE('',#2753,#2756,#1514,.T.);
#3243=EDGE_CURVE('',#2757,#2753,#1515,.T.);
#3244=EDGE_CURVE('',#2758,#2756,#1516,.T.);
#3245=EDGE_CURVE('',#2757,#2758,#1517,.T.);
#3246=EDGE_CURVE('',#2759,#2757,#1518,.T.);
#3247=EDGE_CURVE('',#2760,#2758,#1519,.T.);
#3248=EDGE_CURVE('',#2759,#2760,#1520,.T.);
#3249=EDGE_CURVE('',#2754,#2759,#1521,.T.);
#3250=EDGE_CURVE('',#2755,#2760,#1522,.T.);
#3251=EDGE_CURVE('',#2761,#2761,#2623,.T.);
#3252=EDGE_CURVE('',#2761,#2762,#1523,.T.);
#3253=EDGE_CURVE('',#2762,#2762,#2624,.T.);
#3254=EDGE_CURVE('',#2763,#2763,#2625,.T.);
#3255=EDGE_CURVE('',#2763,#2764,#1524,.T.);
#3256=EDGE_CURVE('',#2764,#2764,#2626,.T.);
#3257=EDGE_CURVE('',#2765,#2765,#2627,.T.);
#3258=EDGE_CURVE('',#2765,#2766,#1525,.T.);
#3259=EDGE_CURVE('',#2766,#2766,#2628,.T.);
#3260=EDGE_CURVE('',#2767,#2767,#2629,.T.);
#3261=EDGE_CURVE('',#2767,#2768,#1526,.T.);
#3262=EDGE_CURVE('',#2768,#2768,#2630,.T.);
#3263=EDGE_CURVE('',#2769,#2770,#1527,.T.);
#3264=EDGE_CURVE('',#2769,#2771,#1528,.T.);
#3265=EDGE_CURVE('',#2772,#2771,#1529,.T.);
#3266=EDGE_CURVE('',#2770,#2772,#1530,.T.);
#3267=EDGE_CURVE('',#2773,#2769,#1531,.T.);
#3268=EDGE_CURVE('',#2774,#2773,#1532,.T.);
#3269=EDGE_CURVE('',#2771,#2774,#1533,.T.);
#3270=EDGE_CURVE('',#2775,#2772,#1534,.T.);
#3271=EDGE_CURVE('',#2775,#2776,#1535,.T.);
#3272=EDGE_CURVE('',#2776,#2770,#1536,.T.);
#3273=EDGE_CURVE('',#2774,#2777,#1537,.T.);
#3274=EDGE_CURVE('',#2777,#2778,#1538,.T.);
#3275=EDGE_CURVE('',#2778,#2779,#1539,.T.);
#3276=EDGE_CURVE('',#2779,#2780,#1540,.T.);
#3277=EDGE_CURVE('',#2780,#2781,#1541,.T.);
#3278=EDGE_CURVE('',#2781,#2782,#1542,.T.);
#3279=EDGE_CURVE('',#2782,#2783,#1543,.T.);
#3280=EDGE_CURVE('',#2783,#2784,#1544,.T.);
#3281=EDGE_CURVE('',#2784,#2775,#1545,.T.);
#3282=EDGE_CURVE('',#2785,#2786,#1546,.T.);
#3283=EDGE_CURVE('',#2785,#2784,#1547,.T.);
#3284=EDGE_CURVE('',#2786,#2783,#1548,.T.);
#3285=EDGE_CURVE('',#2776,#2785,#1549,.T.);
#3286=EDGE_CURVE('',#2782,#2787,#1550,.T.);
#3287=EDGE_CURVE('',#2787,#2786,#1551,.T.);
#3288=EDGE_CURVE('',#2788,#2789,#1552,.T.);
#3289=EDGE_CURVE('',#2788,#2778,#1553,.T.);
#3290=EDGE_CURVE('',#2789,#2777,#1554,.T.);
#3291=EDGE_CURVE('',#2790,#2788,#1555,.T.);
#3292=EDGE_CURVE('',#2779,#2790,#1556,.T.);
#3293=EDGE_CURVE('',#2773,#2789,#1557,.T.);
#3294=EDGE_CURVE('',#2791,#2781,#1558,.T.);
#3295=EDGE_CURVE('',#2787,#2791,#1559,.T.);
#3296=EDGE_CURVE('',#2792,#2780,#1560,.T.);
#3297=EDGE_CURVE('',#2791,#2792,#1561,.T.);
#3298=EDGE_CURVE('',#2790,#2792,#1562,.T.);
#3299=EDGE_CURVE('',#2793,#2793,#2631,.T.);
#3300=EDGE_CURVE('',#2793,#2794,#1563,.T.);
#3301=EDGE_CURVE('',#2794,#2794,#2632,.T.);
#3302=EDGE_CURVE('',#2795,#2795,#2633,.T.);
#3303=EDGE_CURVE('',#2795,#2796,#1564,.T.);
#3304=EDGE_CURVE('',#2796,#2796,#2634,.T.);
#3305=EDGE_CURVE('',#2797,#2797,#2635,.T.);
#3306=EDGE_CURVE('',#2797,#2798,#1565,.T.);
#3307=EDGE_CURVE('',#2798,#2798,#2636,.T.);
#3308=EDGE_CURVE('',#2799,#2800,#1566,.T.);
#3309=EDGE_CURVE('',#2800,#2801,#1567,.T.);
#3310=EDGE_CURVE('',#2802,#2801,#1568,.T.);
#3311=EDGE_CURVE('',#2799,#2802,#1569,.T.);
#3312=EDGE_CURVE('',#2803,#2799,#1570,.T.);
#3313=EDGE_CURVE('',#2804,#2802,#1571,.T.);
#3314=EDGE_CURVE('',#2803,#2804,#1572,.T.);
#3315=EDGE_CURVE('',#2805,#2803,#1573,.T.);
#3316=EDGE_CURVE('',#2806,#2804,#1574,.T.);
#3317=EDGE_CURVE('',#2805,#2806,#1575,.T.);
#3318=EDGE_CURVE('',#2807,#2805,#1576,.T.);
#3319=EDGE_CURVE('',#2808,#2806,#1577,.T.);
#3320=EDGE_CURVE('',#2807,#2808,#1578,.T.);
#3321=EDGE_CURVE('',#2809,#2807,#1579,.T.);
#3322=EDGE_CURVE('',#2810,#2808,#1580,.T.);
#3323=EDGE_CURVE('',#2809,#2810,#1581,.T.);
#3324=EDGE_CURVE('',#2800,#2809,#1582,.T.);
#3325=EDGE_CURVE('',#2801,#2810,#1583,.T.);
#3326=EDGE_CURVE('',#2811,#2811,#2637,.T.);
#3327=EDGE_CURVE('',#2811,#2812,#1584,.T.);
#3328=EDGE_CURVE('',#2812,#2812,#2638,.T.);
#3329=EDGE_CURVE('',#2813,#2813,#2639,.T.);
#3330=EDGE_CURVE('',#2813,#2814,#1585,.T.);
#3331=EDGE_CURVE('',#2814,#2814,#2640,.T.);
#3332=EDGE_CURVE('',#2815,#2815,#2641,.T.);
#3333=EDGE_CURVE('',#2815,#2816,#1586,.T.);
#3334=EDGE_CURVE('',#2816,#2816,#2642,.T.);
#3335=EDGE_CURVE('',#2817,#2818,#1587,.T.);
#3336=EDGE_CURVE('',#2818,#2819,#1588,.T.);
#3337=EDGE_CURVE('',#2820,#2819,#1589,.T.);
#3338=EDGE_CURVE('',#2817,#2820,#1590,.T.);
#3339=EDGE_CURVE('',#2821,#2817,#1591,.T.);
#3340=EDGE_CURVE('',#2822,#2820,#1592,.T.);
#3341=EDGE_CURVE('',#2821,#2822,#1593,.T.);
#3342=EDGE_CURVE('',#2823,#2821,#1594,.T.);
#3343=EDGE_CURVE('',#2824,#2822,#1595,.T.);
#3344=EDGE_CURVE('',#2823,#2824,#1596,.T.);
#3345=EDGE_CURVE('',#2825,#2823,#1597,.T.);
#3346=EDGE_CURVE('',#2826,#2824,#1598,.T.);
#3347=EDGE_CURVE('',#2825,#2826,#1599,.T.);
#3348=EDGE_CURVE('',#2827,#2825,#1600,.T.);
#3349=EDGE_CURVE('',#2828,#2826,#1601,.T.);
#3350=EDGE_CURVE('',#2827,#2828,#1602,.T.);
#3351=EDGE_CURVE('',#2818,#2827,#1603,.T.);
#3352=EDGE_CURVE('',#2819,#2828,#1604,.T.);
#3353=EDGE_CURVE('',#2829,#2829,#2643,.T.);
#3354=EDGE_CURVE('',#2829,#2830,#1605,.T.);
#3355=EDGE_CURVE('',#2830,#2830,#2644,.T.);
#3356=EDGE_CURVE('',#2831,#2831,#2645,.T.);
#3357=EDGE_CURVE('',#2831,#2832,#1606,.T.);
#3358=EDGE_CURVE('',#2832,#2832,#2646,.T.);
#3359=EDGE_CURVE('',#2833,#2834,#1607,.T.);
#3360=EDGE_CURVE('',#2834,#2835,#1608,.T.);
#3361=EDGE_CURVE('',#2836,#2835,#1609,.T.);
#3362=EDGE_CURVE('',#2833,#2836,#1610,.T.);
#3363=EDGE_CURVE('',#2837,#2833,#1611,.T.);
#3364=EDGE_CURVE('',#2838,#2836,#1612,.T.);
#3365=EDGE_CURVE('',#2837,#2838,#1613,.T.);
#3366=EDGE_CURVE('',#2839,#2837,#1614,.T.);
#3367=EDGE_CURVE('',#2840,#2838,#1615,.T.);
#3368=EDGE_CURVE('',#2839,#2840,#1616,.T.);
#3369=EDGE_CURVE('',#2834,#2839,#1617,.T.);
#3370=EDGE_CURVE('',#2835,#2840,#1618,.T.);
#3371=EDGE_CURVE('',#2841,#2841,#2647,.T.);
#3372=EDGE_CURVE('',#2841,#2842,#1619,.T.);
#3373=EDGE_CURVE('',#2843,#2842,#425,.T.);
#3374=EDGE_CURVE('',#2844,#2843,#426,.T.);
#3375=EDGE_CURVE('',#2844,#2845,#1620,.T.);
#3376=EDGE_CURVE('',#2845,#2845,#2648,.T.);
#3377=EDGE_CURVE('',#2846,#2844,#427,.T.);
#3378=EDGE_CURVE('',#2842,#2846,#428,.T.);
#3379=EDGE_CURVE('',#2847,#2848,#429,.T.);
#3380=EDGE_CURVE('',#2848,#2847,#430,.T.);
#3381=EDGE_CURVE('',#2849,#2849,#2649,.T.);
#3382=EDGE_CURVE('',#2849,#2850,#1621,.T.);
#3383=EDGE_CURVE('',#2851,#2850,#431,.T.);
#3384=EDGE_CURVE('',#2852,#2851,#432,.T.);
#3385=EDGE_CURVE('',#2852,#2853,#1622,.T.);
#3386=EDGE_CURVE('',#2853,#2853,#2650,.T.);
#3387=EDGE_CURVE('',#2854,#2852,#433,.T.);
#3388=EDGE_CURVE('',#2850,#2854,#434,.T.);
#3389=EDGE_CURVE('',#2855,#2856,#435,.T.);
#3390=EDGE_CURVE('',#2856,#2855,#436,.T.);
#3391=EDGE_CURVE('',#2848,#2851,#1623,.T.);
#3392=EDGE_CURVE('',#2857,#2858,#437,.T.);
#3393=EDGE_CURVE('',#2858,#2843,#1624,.T.);
#3394=EDGE_CURVE('',#2858,#2857,#438,.T.);
#3395=EDGE_CURVE('',#2859,#2859,#2651,.T.);
#3396=EDGE_CURVE('',#2859,#2860,#1625,.T.);
#3397=EDGE_CURVE('',#2861,#2860,#439,.T.);
#3398=EDGE_CURVE('',#2861,#2862,#1626,.T.);
#3399=EDGE_CURVE('',#2862,#2862,#2652,.T.);
#3400=EDGE_CURVE('',#2863,#2861,#440,.T.);
#3401=EDGE_CURVE('',#2860,#2863,#441,.T.);
#3402=EDGE_CURVE('',#2864,#2864,#2653,.T.);
#3403=EDGE_CURVE('',#2864,#2865,#1627,.T.);
#3404=EDGE_CURVE('',#2866,#2865,#442,.T.);
#3405=EDGE_CURVE('',#2866,#2867,#1628,.T.);
#3406=EDGE_CURVE('',#2867,#2867,#2654,.T.);
#3407=EDGE_CURVE('',#2868,#2866,#443,.T.);
#3408=EDGE_CURVE('',#2865,#2868,#444,.T.);
#3409=EDGE_CURVE('',#2869,#2870,#445,.T.);
#3410=EDGE_CURVE('',#2870,#2869,#446,.T.);
#3411=EDGE_CURVE('',#2856,#2866,#1629,.T.);
#3412=EDGE_CURVE('',#2871,#2871,#2655,.T.);
#3413=EDGE_CURVE('',#2871,#2861,#1630,.T.);
#3414=EDGE_CURVE('',#2872,#2873,#1631,.T.);
#3415=EDGE_CURVE('',#2872,#2874,#1632,.T.);
#3416=EDGE_CURVE('',#2875,#2874,#1633,.T.);
#3417=EDGE_CURVE('',#2873,#2875,#1634,.T.);
#3418=EDGE_CURVE('',#2876,#2872,#1635,.T.);
#3419=EDGE_CURVE('',#2876,#2877,#1636,.T.);
#3420=EDGE_CURVE('',#2874,#2877,#1637,.T.);
#3421=EDGE_CURVE('',#2878,#2876,#1638,.T.);
#3422=EDGE_CURVE('',#2878,#2879,#1639,.T.);
#3423=EDGE_CURVE('',#2877,#2879,#1640,.T.);
#3424=EDGE_CURVE('',#2880,#2878,#1641,.T.);
#3425=EDGE_CURVE('',#2880,#2881,#1642,.T.);
#3426=EDGE_CURVE('',#2879,#2881,#1643,.T.);
#3427=EDGE_CURVE('',#2882,#2880,#1644,.T.);
#3428=EDGE_CURVE('',#2882,#2883,#1645,.T.);
#3429=EDGE_CURVE('',#2881,#2883,#1646,.T.);
#3430=EDGE_CURVE('',#2884,#2882,#1647,.T.);
#3431=EDGE_CURVE('',#2884,#2885,#1648,.T.);
#3432=EDGE_CURVE('',#2883,#2885,#1649,.T.);
#3433=EDGE_CURVE('',#2886,#2884,#1650,.T.);
#3434=EDGE_CURVE('',#2886,#2887,#1651,.T.);
#3435=EDGE_CURVE('',#2885,#2887,#1652,.T.);
#3436=EDGE_CURVE('',#2888,#2886,#1653,.T.);
#3437=EDGE_CURVE('',#2888,#2889,#1654,.T.);
#3438=EDGE_CURVE('',#2887,#2889,#1655,.T.);
#3439=EDGE_CURVE('',#2890,#2888,#1656,.T.);
#3440=EDGE_CURVE('',#2891,#2890,#1657,.T.);
#3441=EDGE_CURVE('',#2889,#2891,#1658,.T.);
#3442=EDGE_CURVE('',#2892,#2893,#1659,.T.);
#3443=EDGE_CURVE('',#2892,#2894,#1660,.T.);
#3444=EDGE_CURVE('',#2895,#2894,#1661,.T.);
#3445=EDGE_CURVE('',#2893,#2895,#1662,.T.);
#3446=EDGE_CURVE('',#2896,#2892,#1663,.T.);
#3447=EDGE_CURVE('',#2896,#2897,#1664,.T.);
#3448=EDGE_CURVE('',#2894,#2897,#1665,.T.);
#3449=EDGE_CURVE('',#2898,#2896,#1666,.T.);
#3450=EDGE_CURVE('',#2898,#2899,#1667,.T.);
#3451=EDGE_CURVE('',#2897,#2899,#1668,.T.);
#3452=EDGE_CURVE('',#2900,#2898,#1669,.T.);
#3453=EDGE_CURVE('',#2900,#2901,#1670,.T.);
#3454=EDGE_CURVE('',#2899,#2901,#1671,.T.);
#3455=EDGE_CURVE('',#2902,#2900,#1672,.T.);
#3456=EDGE_CURVE('',#2902,#2903,#1673,.T.);
#3457=EDGE_CURVE('',#2901,#2903,#1674,.T.);
#3458=EDGE_CURVE('',#2904,#2902,#1675,.T.);
#3459=EDGE_CURVE('',#2904,#2905,#1676,.T.);
#3460=EDGE_CURVE('',#2903,#2905,#1677,.T.);
#3461=EDGE_CURVE('',#2906,#2904,#1678,.T.);
#3462=EDGE_CURVE('',#2906,#2907,#1679,.T.);
#3463=EDGE_CURVE('',#2905,#2907,#1680,.T.);
#3464=EDGE_CURVE('',#2908,#2906,#1681,.T.);
#3465=EDGE_CURVE('',#2908,#2909,#1682,.T.);
#3466=EDGE_CURVE('',#2907,#2909,#1683,.T.);
#3467=EDGE_CURVE('',#2910,#2908,#1684,.T.);
#3468=EDGE_CURVE('',#2911,#2910,#1685,.T.);
#3469=EDGE_CURVE('',#2909,#2911,#1686,.T.);
#3470=EDGE_CURVE('',#2912,#2913,#1687,.T.);
#3471=EDGE_CURVE('',#2912,#2914,#1688,.T.);
#3472=EDGE_CURVE('',#2915,#2914,#1689,.T.);
#3473=EDGE_CURVE('',#2913,#2915,#1690,.T.);
#3474=EDGE_CURVE('',#2916,#2912,#1691,.T.);
#3475=EDGE_CURVE('',#2916,#2917,#1692,.T.);
#3476=EDGE_CURVE('',#2914,#2917,#1693,.T.);
#3477=EDGE_CURVE('',#2918,#2916,#1694,.T.);
#3478=EDGE_CURVE('',#2918,#2919,#1695,.T.);
#3479=EDGE_CURVE('',#2917,#2919,#1696,.T.);
#3480=EDGE_CURVE('',#2920,#2918,#1697,.T.);
#3481=EDGE_CURVE('',#2920,#2921,#1698,.T.);
#3482=EDGE_CURVE('',#2919,#2921,#1699,.T.);
#3483=EDGE_CURVE('',#2922,#2920,#1700,.T.);
#3484=EDGE_CURVE('',#2922,#2923,#1701,.T.);
#3485=EDGE_CURVE('',#2921,#2923,#1702,.T.);
#3486=EDGE_CURVE('',#2924,#2922,#1703,.T.);
#3487=EDGE_CURVE('',#2924,#2925,#1704,.T.);
#3488=EDGE_CURVE('',#2923,#2925,#1705,.T.);
#3489=EDGE_CURVE('',#2926,#2924,#1706,.T.);
#3490=EDGE_CURVE('',#2926,#2927,#1707,.T.);
#3491=EDGE_CURVE('',#2925,#2927,#1708,.T.);
#3492=EDGE_CURVE('',#2928,#2926,#1709,.T.);
#3493=EDGE_CURVE('',#2928,#2929,#1710,.T.);
#3494=EDGE_CURVE('',#2927,#2929,#1711,.T.);
#3495=EDGE_CURVE('',#2930,#2928,#1712,.T.);
#3496=EDGE_CURVE('',#2931,#2930,#1713,.T.);
#3497=EDGE_CURVE('',#2929,#2931,#1714,.T.);
#3498=EDGE_CURVE('',#2932,#2933,#1715,.T.);
#3499=EDGE_CURVE('',#2932,#2934,#1716,.T.);
#3500=EDGE_CURVE('',#2935,#2934,#1717,.T.);
#3501=EDGE_CURVE('',#2933,#2935,#1718,.T.);
#3502=EDGE_CURVE('',#2936,#2932,#1719,.T.);
#3503=EDGE_CURVE('',#2936,#2937,#1720,.T.);
#3504=EDGE_CURVE('',#2934,#2937,#1721,.T.);
#3505=EDGE_CURVE('',#2938,#2936,#1722,.T.);
#3506=EDGE_CURVE('',#2938,#2939,#1723,.T.);
#3507=EDGE_CURVE('',#2937,#2939,#1724,.T.);
#3508=EDGE_CURVE('',#2940,#2938,#1725,.T.);
#3509=EDGE_CURVE('',#2940,#2941,#1726,.T.);
#3510=EDGE_CURVE('',#2939,#2941,#1727,.T.);
#3511=EDGE_CURVE('',#2942,#2940,#1728,.T.);
#3512=EDGE_CURVE('',#2942,#2943,#1729,.T.);
#3513=EDGE_CURVE('',#2941,#2943,#1730,.T.);
#3514=EDGE_CURVE('',#2944,#2942,#1731,.T.);
#3515=EDGE_CURVE('',#2944,#2945,#1732,.T.);
#3516=EDGE_CURVE('',#2943,#2945,#1733,.T.);
#3517=EDGE_CURVE('',#2946,#2944,#1734,.T.);
#3518=EDGE_CURVE('',#2946,#2947,#1735,.T.);
#3519=EDGE_CURVE('',#2945,#2947,#1736,.T.);
#3520=EDGE_CURVE('',#2948,#2946,#1737,.T.);
#3521=EDGE_CURVE('',#2948,#2949,#1738,.T.);
#3522=EDGE_CURVE('',#2947,#2949,#1739,.T.);
#3523=EDGE_CURVE('',#2950,#2948,#1740,.T.);
#3524=EDGE_CURVE('',#2951,#2950,#1741,.T.);
#3525=EDGE_CURVE('',#2949,#2951,#1742,.T.);
#3526=EDGE_CURVE('',#2870,#2952,#1743,.T.);
#3527=EDGE_CURVE('',#2952,#2952,#2656,.T.);
#3528=EDGE_CURVE('',#2890,#2953,#1744,.T.);
#3529=EDGE_CURVE('',#2953,#2954,#1745,.T.);
#3530=EDGE_CURVE('',#2891,#2954,#1746,.T.);
#3531=EDGE_CURVE('',#2955,#2875,#1747,.T.);
#3532=EDGE_CURVE('',#2956,#2955,#1748,.T.);
#3533=EDGE_CURVE('',#2956,#2873,#1749,.T.);
#3534=EDGE_CURVE('',#2910,#2956,#1750,.T.);
#3535=EDGE_CURVE('',#2911,#2955,#1751,.T.);
#3536=EDGE_CURVE('',#2957,#2895,#1752,.T.);
#3537=EDGE_CURVE('',#2958,#2957,#1753,.T.);
#3538=EDGE_CURVE('',#2958,#2893,#1754,.T.);
#3539=EDGE_CURVE('',#2930,#2958,#1755,.T.);
#3540=EDGE_CURVE('',#2931,#2957,#1756,.T.);
#3541=EDGE_CURVE('',#2959,#2915,#1757,.T.);
#3542=EDGE_CURVE('',#2960,#2959,#1758,.T.);
#3543=EDGE_CURVE('',#2960,#2913,#1759,.T.);
#3544=EDGE_CURVE('',#2950,#2960,#1760,.T.);
#3545=EDGE_CURVE('',#2951,#2959,#1761,.T.);
#3546=EDGE_CURVE('',#2954,#2935,#1762,.T.);
#3547=EDGE_CURVE('',#2953,#2933,#1763,.T.);
#3548=EDGE_CURVE('',#2961,#2962,#1764,.T.);
#3549=EDGE_CURVE('',#2963,#2961,#1765,.T.);
#3550=EDGE_CURVE('',#2964,#2963,#1766,.T.);
#3551=EDGE_CURVE('',#2965,#2964,#1767,.T.);
#3552=EDGE_CURVE('',#2966,#2965,#1768,.T.);
#3553=EDGE_CURVE('',#2967,#2966,#1769,.T.);
#3554=EDGE_CURVE('',#2968,#2967,#1770,.T.);
#3555=EDGE_CURVE('',#2969,#2968,#1771,.T.);
#3556=EDGE_CURVE('',#2970,#2969,#1772,.T.);
#3557=EDGE_CURVE('',#2971,#2970,#1773,.T.);
#3558=EDGE_CURVE('',#2972,#2971,#1774,.T.);
#3559=EDGE_CURVE('',#2973,#2972,#1775,.T.);
#3560=EDGE_CURVE('',#2974,#2973,#1776,.T.);
#3561=EDGE_CURVE('',#2975,#2974,#1777,.T.);
#3562=EDGE_CURVE('',#2976,#2975,#1778,.T.);
#3563=EDGE_CURVE('',#2977,#2976,#1779,.T.);
#3564=EDGE_CURVE('',#2978,#2977,#1780,.T.);
#3565=EDGE_CURVE('',#2979,#2978,#1781,.T.);
#3566=EDGE_CURVE('',#2980,#2979,#1782,.T.);
#3567=EDGE_CURVE('',#2981,#2980,#1783,.T.);
#3568=EDGE_CURVE('',#2982,#2981,#1784,.T.);
#3569=EDGE_CURVE('',#2983,#2982,#1785,.T.);
#3570=EDGE_CURVE('',#2984,#2983,#1786,.T.);
#3571=EDGE_CURVE('',#2985,#2984,#1787,.T.);
#3572=EDGE_CURVE('',#2986,#2985,#1788,.T.);
#3573=EDGE_CURVE('',#2987,#2986,#1789,.T.);
#3574=EDGE_CURVE('',#2988,#2987,#1790,.T.);
#3575=EDGE_CURVE('',#2989,#2988,#1791,.T.);
#3576=EDGE_CURVE('',#2990,#2989,#1792,.T.);
#3577=EDGE_CURVE('',#2991,#2990,#1793,.T.);
#3578=EDGE_CURVE('',#2992,#2991,#1794,.T.);
#3579=EDGE_CURVE('',#2993,#2992,#1795,.T.);
#3580=EDGE_CURVE('',#2994,#2993,#1796,.T.);
#3581=EDGE_CURVE('',#2995,#2994,#1797,.T.);
#3582=EDGE_CURVE('',#2996,#2995,#1798,.T.);
#3583=EDGE_CURVE('',#2997,#2996,#1799,.T.);
#3584=EDGE_CURVE('',#2998,#2997,#1800,.T.);
#3585=EDGE_CURVE('',#2999,#2998,#1801,.T.);
#3586=EDGE_CURVE('',#3000,#2999,#1802,.T.);
#3587=EDGE_CURVE('',#3001,#3000,#1803,.T.);
#3588=EDGE_CURVE('',#3002,#3001,#1804,.T.);
#3589=EDGE_CURVE('',#3003,#3002,#1805,.T.);
#3590=EDGE_CURVE('',#3004,#3003,#1806,.T.);
#3591=EDGE_CURVE('',#2962,#3004,#1807,.T.);
#3592=EDGE_CURVE('',#3005,#3005,#2657,.T.);
#3593=EDGE_CURVE('',#3006,#2983,#1808,.T.);
#3594=EDGE_CURVE('',#3007,#3006,#1809,.T.);
#3595=EDGE_CURVE('',#3007,#2984,#1810,.T.);
#3596=EDGE_CURVE('',#3008,#2982,#1811,.T.);
#3597=EDGE_CURVE('',#3008,#3006,#1812,.T.);
#3598=EDGE_CURVE('',#2981,#3009,#1813,.T.);
#3599=EDGE_CURVE('',#3009,#3008,#1814,.T.);
#3600=EDGE_CURVE('',#3010,#2980,#1815,.T.);
#3601=EDGE_CURVE('',#3009,#3010,#1816,.T.);
#3602=EDGE_CURVE('',#3011,#2979,#1817,.T.);
#3603=EDGE_CURVE('',#3010,#3011,#1818,.T.);
#3604=EDGE_CURVE('',#3012,#2978,#1819,.T.);
#3605=EDGE_CURVE('',#3011,#3012,#1820,.T.);
#3606=EDGE_CURVE('',#3013,#2977,#1821,.T.);
#3607=EDGE_CURVE('',#3012,#3013,#1822,.T.);
#3608=EDGE_CURVE('',#3014,#2976,#1823,.T.);
#3609=EDGE_CURVE('',#3013,#3014,#1824,.T.);
#3610=EDGE_CURVE('',#3015,#2975,#1825,.T.);
#3611=EDGE_CURVE('',#3014,#3015,#1826,.T.);
#3612=EDGE_CURVE('',#3016,#2974,#1827,.T.);
#3613=EDGE_CURVE('',#3015,#3016,#1828,.T.);
#3614=EDGE_CURVE('',#3017,#2973,#1829,.T.);
#3615=EDGE_CURVE('',#3016,#3017,#1830,.T.);
#3616=EDGE_CURVE('',#3018,#2972,#1831,.T.);
#3617=EDGE_CURVE('',#3017,#3018,#1832,.T.);
#3618=EDGE_CURVE('',#3019,#2971,#1833,.T.);
#3619=EDGE_CURVE('',#3019,#3018,#1834,.T.);
#3620=EDGE_CURVE('',#2970,#3020,#1835,.T.);
#3621=EDGE_CURVE('',#3020,#3019,#1836,.T.);
#3622=EDGE_CURVE('',#3021,#2969,#1837,.T.);
#3623=EDGE_CURVE('',#3020,#3021,#1838,.T.);
#3624=EDGE_CURVE('',#3022,#2968,#1839,.T.);
#3625=EDGE_CURVE('',#3021,#3022,#1840,.T.);
#3626=EDGE_CURVE('',#3023,#2967,#1841,.T.);
#3627=EDGE_CURVE('',#3022,#3023,#1842,.T.);
#3628=EDGE_CURVE('',#3024,#2966,#1843,.T.);
#3629=EDGE_CURVE('',#3023,#3024,#1844,.T.);
#3630=EDGE_CURVE('',#3025,#2965,#1845,.T.);
#3631=EDGE_CURVE('',#3024,#3025,#1846,.T.);
#3632=EDGE_CURVE('',#3026,#2964,#1847,.T.);
#3633=EDGE_CURVE('',#3025,#3026,#1848,.T.);
#3634=EDGE_CURVE('',#3027,#2963,#1849,.T.);
#3635=EDGE_CURVE('',#3026,#3027,#1850,.T.);
#3636=EDGE_CURVE('',#3028,#2961,#1851,.T.);
#3637=EDGE_CURVE('',#3027,#3028,#1852,.T.);
#3638=EDGE_CURVE('',#3029,#2994,#1853,.T.);
#3639=EDGE_CURVE('',#3030,#3029,#1854,.T.);
#3640=EDGE_CURVE('',#3030,#2995,#1855,.T.);
#3641=EDGE_CURVE('',#3031,#3030,#1856,.T.);
#3642=EDGE_CURVE('',#3031,#2996,#1857,.T.);
#3643=EDGE_CURVE('',#3032,#3031,#1858,.T.);
#3644=EDGE_CURVE('',#3032,#2997,#1859,.T.);
#3645=EDGE_CURVE('',#3033,#3032,#1860,.T.);
#3646=EDGE_CURVE('',#3033,#2998,#1861,.T.);
#3647=EDGE_CURVE('',#3034,#3033,#1862,.T.);
#3648=EDGE_CURVE('',#3034,#2999,#1863,.T.);
#3649=EDGE_CURVE('',#3035,#3034,#1864,.T.);
#3650=EDGE_CURVE('',#3035,#3000,#1865,.T.);
#3651=EDGE_CURVE('',#3036,#3035,#1866,.T.);
#3652=EDGE_CURVE('',#3036,#3001,#1867,.T.);
#3653=EDGE_CURVE('',#3037,#3036,#1868,.T.);
#3654=EDGE_CURVE('',#3037,#3002,#1869,.T.);
#3655=EDGE_CURVE('',#3038,#3037,#1870,.T.);
#3656=EDGE_CURVE('',#3003,#3038,#1871,.T.);
#3657=EDGE_CURVE('',#3039,#3007,#1872,.T.);
#3658=EDGE_CURVE('',#3039,#2985,#1873,.T.);
#3659=EDGE_CURVE('',#3040,#3039,#1874,.T.);
#3660=EDGE_CURVE('',#3040,#2986,#1875,.T.);
#3661=EDGE_CURVE('',#3041,#3040,#1876,.T.);
#3662=EDGE_CURVE('',#3041,#2987,#1877,.T.);
#3663=EDGE_CURVE('',#3042,#3041,#1878,.T.);
#3664=EDGE_CURVE('',#3042,#2988,#1879,.T.);
#3665=EDGE_CURVE('',#3043,#3042,#1880,.T.);
#3666=EDGE_CURVE('',#3043,#2989,#1881,.T.);
#3667=EDGE_CURVE('',#3044,#3043,#1882,.T.);
#3668=EDGE_CURVE('',#3044,#2990,#1883,.T.);
#3669=EDGE_CURVE('',#3045,#3044,#1884,.T.);
#3670=EDGE_CURVE('',#3045,#2991,#1885,.T.);
#3671=EDGE_CURVE('',#3046,#3045,#1886,.T.);
#3672=EDGE_CURVE('',#2992,#3046,#1887,.T.);
#3673=EDGE_CURVE('',#3047,#2962,#1888,.T.);
#3674=EDGE_CURVE('',#3028,#3047,#1889,.T.);
#3675=EDGE_CURVE('',#3048,#3048,#2658,.T.);
#3676=EDGE_CURVE('',#3048,#3005,#1890,.T.);
#3677=EDGE_CURVE('',#3038,#3049,#1891,.T.);
#3678=EDGE_CURVE('',#3049,#3004,#1892,.T.);
#3679=EDGE_CURVE('',#3050,#2993,#1893,.T.);
#3680=EDGE_CURVE('',#3050,#3029,#1894,.T.);
#3681=EDGE_CURVE('',#3046,#3050,#1895,.T.);
#3682=EDGE_CURVE('',#3049,#3047,#1896,.T.);
#3683=EDGE_CURVE('',#3051,#3052,#1897,.T.);
#3684=EDGE_CURVE('',#3052,#3053,#1898,.T.);
#3685=EDGE_CURVE('',#3053,#3054,#1899,.T.);
#3686=EDGE_CURVE('',#3051,#3054,#1900,.T.);
#3687=EDGE_CURVE('',#3052,#3055,#1901,.T.);
#3688=EDGE_CURVE('',#3055,#3056,#1902,.T.);
#3689=EDGE_CURVE('',#3056,#3053,#1903,.T.);
#3690=EDGE_CURVE('',#3055,#3057,#1904,.T.);
#3691=EDGE_CURVE('',#3057,#3058,#1905,.T.);
#3692=EDGE_CURVE('',#3058,#3056,#1906,.T.);
#3693=EDGE_CURVE('',#3057,#3059,#1907,.T.);
#3694=EDGE_CURVE('',#3059,#3060,#1908,.T.);
#3695=EDGE_CURVE('',#3060,#3058,#1909,.T.);
#3696=EDGE_CURVE('',#3059,#3061,#1910,.T.);
#3697=EDGE_CURVE('',#3061,#3062,#1911,.T.);
#3698=EDGE_CURVE('',#3062,#3060,#1912,.T.);
#3699=EDGE_CURVE('',#3061,#3051,#1913,.T.);
#3700=EDGE_CURVE('',#3054,#3062,#1914,.T.);
#3701=EDGE_CURVE('',#3063,#3063,#2659,.T.);
#3702=EDGE_CURVE('',#3064,#3064,#2660,.T.);
#3703=EDGE_CURVE('',#3063,#3065,#1915,.T.);
#3704=EDGE_CURVE('',#3065,#3065,#2661,.T.);
#3705=EDGE_CURVE('',#3066,#3066,#2662,.T.);
#3706=EDGE_CURVE('',#3067,#3067,#2663,.T.);
#3707=EDGE_CURVE('',#3067,#3066,#1916,.T.);
#3708=EDGE_CURVE('',#3068,#3068,#2664,.T.);
#3709=EDGE_CURVE('',#3068,#3067,#1917,.T.);
#3710=EDGE_CURVE('',#3069,#3069,#2665,.T.);
#3711=EDGE_CURVE('',#3069,#3068,#1918,.T.);
#3712=EDGE_CURVE('',#3070,#3070,#2666,.T.);
#3713=EDGE_CURVE('',#3071,#3071,#2667,.F.);
#3714=EDGE_CURVE('',#3071,#3070,#1919,.T.);
#3715=EDGE_CURVE('',#3064,#3071,#1920,.T.);
#3716=EDGE_CURVE('',#3072,#3072,#2668,.T.);
#3717=EDGE_CURVE('',#3073,#3073,#2669,.T.);
#3718=EDGE_CURVE('',#3073,#3072,#1921,.T.);
#3719=EDGE_CURVE('',#3074,#3074,#2670,.T.);
#3720=EDGE_CURVE('',#3074,#3073,#1922,.T.);
#3721=EDGE_CURVE('',#3075,#3075,#2671,.T.);
#3722=EDGE_CURVE('',#3075,#3074,#1923,.T.);
#3723=EDGE_CURVE('',#3076,#3076,#2672,.T.);
#3724=EDGE_CURVE('',#3077,#3077,#2673,.F.);
#3725=EDGE_CURVE('',#3077,#3076,#1924,.T.);
#3726=EDGE_CURVE('',#3078,#3078,#2674,.F.);
#3727=EDGE_CURVE('',#3078,#3077,#1925,.T.);
#3728=EDGE_CURVE('',#3079,#3079,#2675,.T.);
#3729=EDGE_CURVE('',#3079,#3078,#1926,.T.);
#3730=EDGE_CURVE('',#3080,#3081,#1927,.T.);
#3731=EDGE_CURVE('',#3081,#3082,#1928,.T.);
#3732=EDGE_CURVE('',#3082,#3083,#1929,.T.);
#3733=EDGE_CURVE('',#3080,#3083,#1930,.T.);
#3734=EDGE_CURVE('',#3081,#3084,#1931,.T.);
#3735=EDGE_CURVE('',#3084,#3085,#1932,.T.);
#3736=EDGE_CURVE('',#3085,#3082,#1933,.T.);
#3737=EDGE_CURVE('',#3084,#3086,#1934,.T.);
#3738=EDGE_CURVE('',#3086,#3087,#1935,.T.);
#3739=EDGE_CURVE('',#3087,#3085,#1936,.T.);
#3740=EDGE_CURVE('',#3086,#3088,#1937,.T.);
#3741=EDGE_CURVE('',#3088,#3089,#1938,.T.);
#3742=EDGE_CURVE('',#3089,#3087,#1939,.T.);
#3743=EDGE_CURVE('',#3088,#3090,#1940,.T.);
#3744=EDGE_CURVE('',#3090,#3091,#1941,.T.);
#3745=EDGE_CURVE('',#3091,#3089,#1942,.T.);
#3746=EDGE_CURVE('',#3090,#3080,#1943,.T.);
#3747=EDGE_CURVE('',#3083,#3091,#1944,.T.);
#3748=EDGE_CURVE('',#3092,#3093,#1945,.T.);
#3749=EDGE_CURVE('',#3094,#3092,#1946,.T.);
#3750=EDGE_CURVE('',#3095,#3094,#1947,.T.);
#3751=EDGE_CURVE('',#3093,#3095,#1948,.T.);
#3752=EDGE_CURVE('',#3094,#3096,#1949,.T.);
#3753=EDGE_CURVE('',#3097,#3096,#1950,.T.);
#3754=EDGE_CURVE('',#3095,#3097,#1951,.T.);
#3755=EDGE_CURVE('',#3096,#3098,#1952,.T.);
#3756=EDGE_CURVE('',#3098,#3099,#1953,.T.);
#3757=EDGE_CURVE('',#3099,#3097,#1954,.T.);
#3758=EDGE_CURVE('',#3100,#3100,#2676,.T.);
#3759=EDGE_CURVE('',#3101,#3092,#1955,.T.);
#3760=EDGE_CURVE('',#3102,#3101,#1956,.T.);
#3761=EDGE_CURVE('',#3102,#3103,#1957,.T.);
#3762=EDGE_CURVE('',#3104,#3103,#1958,.T.);
#3763=EDGE_CURVE('',#3104,#3105,#1959,.T.);
#3764=EDGE_CURVE('',#3105,#3106,#1960,.T.);
#3765=EDGE_CURVE('',#3106,#3098,#1961,.T.);
#3766=EDGE_CURVE('',#3106,#3107,#1962,.T.);
#3767=EDGE_CURVE('',#3107,#3099,#1963,.T.);
#3768=EDGE_CURVE('',#3108,#3105,#1964,.T.);
#3769=EDGE_CURVE('',#3107,#3108,#1965,.T.);
#3770=EDGE_CURVE('',#3109,#3108,#1966,.T.);
#3771=EDGE_CURVE('',#3110,#3109,#1967,.T.);
#3772=EDGE_CURVE('',#3110,#3111,#1968,.T.);
#3773=EDGE_CURVE('',#3112,#3111,#1969,.T.);
#3774=EDGE_CURVE('',#3112,#3093,#1970,.T.);
#3775=EDGE_CURVE('',#3109,#3104,#1971,.T.);
#3776=EDGE_CURVE('',#3103,#3113,#1972,.T.);
#3777=EDGE_CURVE('',#3113,#3114,#399,.T.);
#3778=EDGE_CURVE('',#3114,#3110,#1973,.T.);
#3779=EDGE_CURVE('',#3115,#3113,#2677,.F.);
#3780=EDGE_CURVE('',#3115,#3100,#1974,.T.);
#3781=EDGE_CURVE('',#3116,#3115,#2678,.F.);
#3782=EDGE_CURVE('',#3117,#3116,#400,.T.);
#3783=EDGE_CURVE('',#3114,#3117,#2679,.F.);
#3784=EDGE_CURVE('',#3116,#3102,#1975,.T.);
#3785=EDGE_CURVE('',#3111,#3117,#1976,.T.);
#3786=EDGE_CURVE('',#3101,#3112,#1977,.T.);
#3787=EDGE_CURVE('',#3118,#3118,#2680,.T.);
#3788=EDGE_CURVE('',#3118,#3119,#1978,.T.);
#3789=EDGE_CURVE('',#3119,#3119,#2681,.T.);
#3790=EDGE_CURVE('',#3119,#3120,#1979,.T.);
#3791=EDGE_CURVE('',#3120,#3120,#2682,.T.);
#3792=EDGE_CURVE('',#3121,#3121,#2683,.T.);
#3793=EDGE_CURVE('',#3121,#3122,#1980,.T.);
#3794=EDGE_CURVE('',#3122,#3122,#2684,.T.);
#3795=EDGE_CURVE('',#3123,#3124,#1981,.T.);
#3796=EDGE_CURVE('',#3124,#3125,#1982,.T.);
#3797=EDGE_CURVE('',#3125,#3126,#1983,.T.);
#3798=EDGE_CURVE('',#3123,#3126,#1984,.T.);
#3799=EDGE_CURVE('',#3124,#3127,#1985,.T.);
#3800=EDGE_CURVE('',#3127,#3128,#1986,.T.);
#3801=EDGE_CURVE('',#3128,#3125,#1987,.T.);
#3802=EDGE_CURVE('',#3127,#3129,#1988,.T.);
#3803=EDGE_CURVE('',#3129,#3130,#1989,.T.);
#3804=EDGE_CURVE('',#3130,#3128,#1990,.T.);
#3805=EDGE_CURVE('',#3129,#3131,#1991,.T.);
#3806=EDGE_CURVE('',#3131,#3132,#1992,.T.);
#3807=EDGE_CURVE('',#3132,#3130,#1993,.T.);
#3808=EDGE_CURVE('',#3131,#3133,#1994,.T.);
#3809=EDGE_CURVE('',#3133,#3134,#1995,.T.);
#3810=EDGE_CURVE('',#3134,#3132,#1996,.T.);
#3811=EDGE_CURVE('',#3133,#3123,#1997,.T.);
#3812=EDGE_CURVE('',#3126,#3134,#1998,.T.);
#3813=EDGE_CURVE('',#3135,#3135,#2685,.T.);
#3814=EDGE_CURVE('',#3136,#3136,#2686,.T.);
#3815=EDGE_CURVE('',#3137,#3137,#2687,.T.);
#3816=EDGE_CURVE('',#3137,#3136,#1999,.T.);
#3817=EDGE_CURVE('',#3138,#3138,#2688,.T.);
#3818=EDGE_CURVE('',#3138,#3137,#2000,.T.);
#3819=EDGE_CURVE('',#3139,#3139,#2689,.T.);
#3820=EDGE_CURVE('',#3139,#3138,#2001,.T.);
#3821=EDGE_CURVE('',#3140,#3140,#2690,.T.);
#3822=EDGE_CURVE('',#3141,#3141,#2691,.F.);
#3823=EDGE_CURVE('',#3141,#3140,#2002,.T.);
#3824=EDGE_CURVE('',#3135,#3141,#2003,.T.);
#3825=EDGE_CURVE('',#3142,#3142,#2692,.T.);
#3826=EDGE_CURVE('',#3142,#3143,#2004,.T.);
#3827=EDGE_CURVE('',#3143,#3143,#2693,.T.);
#3828=EDGE_CURVE('',#3143,#3144,#2005,.T.);
#3829=EDGE_CURVE('',#3144,#3144,#2694,.T.);
#3830=EDGE_CURVE('',#3145,#3145,#2695,.T.);
#3831=EDGE_CURVE('',#3145,#3146,#2006,.T.);
#3832=EDGE_CURVE('',#3146,#3146,#2696,.T.);
#3833=EDGE_CURVE('',#3147,#3147,#2697,.T.);
#3834=EDGE_CURVE('',#3148,#3148,#2698,.T.);
#3835=EDGE_CURVE('',#3148,#3147,#2007,.T.);
#3836=EDGE_CURVE('',#3149,#3149,#2699,.T.);
#3837=EDGE_CURVE('',#3149,#3148,#2008,.T.);
#3838=EDGE_CURVE('',#3150,#3150,#2700,.T.);
#3839=EDGE_CURVE('',#3150,#3149,#2009,.T.);
#3840=EDGE_CURVE('',#3151,#3151,#2701,.T.);
#3841=EDGE_CURVE('',#3152,#3152,#2702,.F.);
#3842=EDGE_CURVE('',#3152,#3151,#2010,.T.);
#3843=EDGE_CURVE('',#3153,#3153,#2703,.F.);
#3844=EDGE_CURVE('',#3153,#3152,#2011,.T.);
#3845=EDGE_CURVE('',#3154,#3154,#2704,.T.);
#3846=EDGE_CURVE('',#3154,#3153,#2012,.T.);
#3847=EDGE_CURVE('',#3155,#3156,#2013,.T.);
#3848=EDGE_CURVE('',#3156,#3157,#2014,.T.);
#3849=EDGE_CURVE('',#3157,#3158,#2015,.T.);
#3850=EDGE_CURVE('',#3155,#3158,#2016,.T.);
#3851=EDGE_CURVE('',#3156,#3159,#2017,.T.);
#3852=EDGE_CURVE('',#3159,#3160,#2018,.T.);
#3853=EDGE_CURVE('',#3160,#3157,#2019,.T.);
#3854=EDGE_CURVE('',#3159,#3161,#2020,.T.);
#3855=EDGE_CURVE('',#3161,#3162,#2021,.T.);
#3856=EDGE_CURVE('',#3162,#3160,#2022,.T.);
#3857=EDGE_CURVE('',#3161,#3163,#2023,.T.);
#3858=EDGE_CURVE('',#3163,#3164,#2024,.T.);
#3859=EDGE_CURVE('',#3164,#3162,#2025,.T.);
#3860=EDGE_CURVE('',#3163,#3165,#2026,.T.);
#3861=EDGE_CURVE('',#3165,#3166,#2027,.T.);
#3862=EDGE_CURVE('',#3166,#3164,#2028,.T.);
#3863=EDGE_CURVE('',#3165,#3155,#2029,.T.);
#3864=EDGE_CURVE('',#3158,#3166,#2030,.T.);
#3865=ORIENTED_EDGE('',*,*,#3167,.F.);
#3866=ORIENTED_EDGE('',*,*,#3168,.T.);
#3867=ORIENTED_EDGE('',*,*,#3169,.T.);
#3868=ORIENTED_EDGE('',*,*,#3168,.F.);
#3869=ORIENTED_EDGE('',*,*,#3170,.F.);
#3870=ORIENTED_EDGE('',*,*,#3171,.T.);
#3871=ORIENTED_EDGE('',*,*,#3172,.T.);
#3872=ORIENTED_EDGE('',*,*,#3171,.F.);
#3873=ORIENTED_EDGE('',*,*,#3170,.T.);
#3874=ORIENTED_EDGE('',*,*,#3167,.T.);
#3875=ORIENTED_EDGE('',*,*,#3172,.F.);
#3876=ORIENTED_EDGE('',*,*,#3169,.F.);
#3877=ORIENTED_EDGE('',*,*,#3173,.F.);
#3878=ORIENTED_EDGE('',*,*,#3174,.T.);
#3879=ORIENTED_EDGE('',*,*,#3175,.T.);
#3880=ORIENTED_EDGE('',*,*,#3174,.F.);
#3881=ORIENTED_EDGE('',*,*,#3176,.F.);
#3882=ORIENTED_EDGE('',*,*,#3177,.T.);
#3883=ORIENTED_EDGE('',*,*,#3178,.T.);
#3884=ORIENTED_EDGE('',*,*,#3177,.F.);
#3885=ORIENTED_EDGE('',*,*,#3176,.T.);
#3886=ORIENTED_EDGE('',*,*,#3173,.T.);
#3887=ORIENTED_EDGE('',*,*,#3178,.F.);
#3888=ORIENTED_EDGE('',*,*,#3175,.F.);
#3889=ORIENTED_EDGE('',*,*,#3179,.F.);
#3890=ORIENTED_EDGE('',*,*,#3180,.T.);
#3891=ORIENTED_EDGE('',*,*,#3181,.T.);
#3892=ORIENTED_EDGE('',*,*,#3180,.F.);
#3893=ORIENTED_EDGE('',*,*,#3182,.F.);
#3894=ORIENTED_EDGE('',*,*,#3183,.T.);
#3895=ORIENTED_EDGE('',*,*,#3184,.T.);
#3896=ORIENTED_EDGE('',*,*,#3183,.F.);
#3897=ORIENTED_EDGE('',*,*,#3182,.T.);
#3898=ORIENTED_EDGE('',*,*,#3179,.T.);
#3899=ORIENTED_EDGE('',*,*,#3184,.F.);
#3900=ORIENTED_EDGE('',*,*,#3181,.F.);
#3901=ORIENTED_EDGE('',*,*,#3185,.F.);
#3902=ORIENTED_EDGE('',*,*,#3186,.T.);
#3903=ORIENTED_EDGE('',*,*,#3187,.T.);
#3904=ORIENTED_EDGE('',*,*,#3186,.F.);
#3905=ORIENTED_EDGE('',*,*,#3188,.F.);
#3906=ORIENTED_EDGE('',*,*,#3189,.T.);
#3907=ORIENTED_EDGE('',*,*,#3190,.T.);
#3908=ORIENTED_EDGE('',*,*,#3189,.F.);
#3909=ORIENTED_EDGE('',*,*,#3188,.T.);
#3910=ORIENTED_EDGE('',*,*,#3185,.T.);
#3911=ORIENTED_EDGE('',*,*,#3190,.F.);
#3912=ORIENTED_EDGE('',*,*,#3187,.F.);
#3913=ORIENTED_EDGE('',*,*,#3191,.F.);
#3914=ORIENTED_EDGE('',*,*,#3192,.T.);
#3915=ORIENTED_EDGE('',*,*,#3193,.T.);
#3916=ORIENTED_EDGE('',*,*,#3192,.F.);
#3917=ORIENTED_EDGE('',*,*,#3194,.F.);
#3918=ORIENTED_EDGE('',*,*,#3195,.T.);
#3919=ORIENTED_EDGE('',*,*,#3196,.T.);
#3920=ORIENTED_EDGE('',*,*,#3195,.F.);
#3921=ORIENTED_EDGE('',*,*,#3194,.T.);
#3922=ORIENTED_EDGE('',*,*,#3191,.T.);
#3923=ORIENTED_EDGE('',*,*,#3196,.F.);
#3924=ORIENTED_EDGE('',*,*,#3193,.F.);
#3925=ORIENTED_EDGE('',*,*,#3197,.F.);
#3926=ORIENTED_EDGE('',*,*,#3198,.T.);
#3927=ORIENTED_EDGE('',*,*,#3199,.T.);
#3928=ORIENTED_EDGE('',*,*,#3198,.F.);
#3929=ORIENTED_EDGE('',*,*,#3200,.F.);
#3930=ORIENTED_EDGE('',*,*,#3201,.T.);
#3931=ORIENTED_EDGE('',*,*,#3202,.T.);
#3932=ORIENTED_EDGE('',*,*,#3201,.F.);
#3933=ORIENTED_EDGE('',*,*,#3200,.T.);
#3934=ORIENTED_EDGE('',*,*,#3197,.T.);
#3935=ORIENTED_EDGE('',*,*,#3202,.F.);
#3936=ORIENTED_EDGE('',*,*,#3199,.F.);
#3937=ORIENTED_EDGE('',*,*,#3203,.F.);
#3938=ORIENTED_EDGE('',*,*,#3204,.T.);
#3939=ORIENTED_EDGE('',*,*,#3205,.T.);
#3940=ORIENTED_EDGE('',*,*,#3204,.F.);
#3941=ORIENTED_EDGE('',*,*,#3206,.F.);
#3942=ORIENTED_EDGE('',*,*,#3207,.T.);
#3943=ORIENTED_EDGE('',*,*,#3208,.T.);
#3944=ORIENTED_EDGE('',*,*,#3207,.F.);
#3945=ORIENTED_EDGE('',*,*,#3206,.T.);
#3946=ORIENTED_EDGE('',*,*,#3203,.T.);
#3947=ORIENTED_EDGE('',*,*,#3208,.F.);
#3948=ORIENTED_EDGE('',*,*,#3205,.F.);
#3949=ORIENTED_EDGE('',*,*,#3209,.F.);
#3950=ORIENTED_EDGE('',*,*,#3210,.T.);
#3951=ORIENTED_EDGE('',*,*,#3211,.T.);
#3952=ORIENTED_EDGE('',*,*,#3210,.F.);
#3953=ORIENTED_EDGE('',*,*,#3212,.F.);
#3954=ORIENTED_EDGE('',*,*,#3213,.T.);
#3955=ORIENTED_EDGE('',*,*,#3214,.T.);
#3956=ORIENTED_EDGE('',*,*,#3213,.F.);
#3957=ORIENTED_EDGE('',*,*,#3212,.T.);
#3958=ORIENTED_EDGE('',*,*,#3209,.T.);
#3959=ORIENTED_EDGE('',*,*,#3214,.F.);
#3960=ORIENTED_EDGE('',*,*,#3211,.F.);
#3961=ORIENTED_EDGE('',*,*,#3215,.F.);
#3962=ORIENTED_EDGE('',*,*,#3216,.T.);
#3963=ORIENTED_EDGE('',*,*,#3217,.F.);
#3964=ORIENTED_EDGE('',*,*,#3216,.F.);
#3965=ORIENTED_EDGE('',*,*,#3215,.T.);
#3966=ORIENTED_EDGE('',*,*,#3218,.F.);
#3967=ORIENTED_EDGE('',*,*,#3219,.F.);
#3968=ORIENTED_EDGE('',*,*,#3220,.T.);
#3969=ORIENTED_EDGE('',*,*,#3221,.F.);
#3970=ORIENTED_EDGE('',*,*,#3220,.F.);
#3971=ORIENTED_EDGE('',*,*,#3219,.T.);
#3972=ORIENTED_EDGE('',*,*,#3222,.F.);
#3973=ORIENTED_EDGE('',*,*,#3223,.F.);
#3974=ORIENTED_EDGE('',*,*,#3224,.T.);
#3975=ORIENTED_EDGE('',*,*,#3225,.F.);
#3976=ORIENTED_EDGE('',*,*,#3224,.F.);
#3977=ORIENTED_EDGE('',*,*,#3223,.T.);
#3978=ORIENTED_EDGE('',*,*,#3226,.F.);
#3979=ORIENTED_EDGE('',*,*,#3227,.F.);
#3980=ORIENTED_EDGE('',*,*,#3228,.T.);
#3981=ORIENTED_EDGE('',*,*,#3229,.F.);
#3982=ORIENTED_EDGE('',*,*,#3228,.F.);
#3983=ORIENTED_EDGE('',*,*,#3227,.T.);
#3984=ORIENTED_EDGE('',*,*,#3230,.F.);
#3985=ORIENTED_EDGE('',*,*,#3231,.F.);
#3986=ORIENTED_EDGE('',*,*,#3232,.T.);
#3987=ORIENTED_EDGE('',*,*,#3218,.T.);
#3988=ORIENTED_EDGE('',*,*,#3232,.F.);
#3989=ORIENTED_EDGE('',*,*,#3233,.F.);
#3990=ORIENTED_EDGE('',*,*,#3234,.T.);
#3991=ORIENTED_EDGE('',*,*,#3222,.T.);
#3992=ORIENTED_EDGE('',*,*,#3234,.F.);
#3993=ORIENTED_EDGE('',*,*,#3235,.F.);
#3994=ORIENTED_EDGE('',*,*,#3236,.T.);
#3995=ORIENTED_EDGE('',*,*,#3226,.T.);
#3996=ORIENTED_EDGE('',*,*,#3236,.F.);
#3997=ORIENTED_EDGE('',*,*,#3237,.F.);
#3998=ORIENTED_EDGE('',*,*,#3238,.T.);
#3999=ORIENTED_EDGE('',*,*,#3230,.T.);
#4000=ORIENTED_EDGE('',*,*,#3238,.F.);
#4001=ORIENTED_EDGE('',*,*,#3239,.T.);
#4002=ORIENTED_EDGE('',*,*,#3240,.T.);
#4003=ORIENTED_EDGE('',*,*,#3241,.F.);
#4004=ORIENTED_EDGE('',*,*,#3242,.F.);
#4005=ORIENTED_EDGE('',*,*,#3243,.T.);
#4006=ORIENTED_EDGE('',*,*,#3242,.T.);
#4007=ORIENTED_EDGE('',*,*,#3244,.F.);
#4008=ORIENTED_EDGE('',*,*,#3245,.F.);
#4009=ORIENTED_EDGE('',*,*,#3246,.T.);
#4010=ORIENTED_EDGE('',*,*,#3245,.T.);
#4011=ORIENTED_EDGE('',*,*,#3247,.F.);
#4012=ORIENTED_EDGE('',*,*,#3248,.F.);
#4013=ORIENTED_EDGE('',*,*,#3249,.T.);
#4014=ORIENTED_EDGE('',*,*,#3248,.T.);
#4015=ORIENTED_EDGE('',*,*,#3250,.F.);
#4016=ORIENTED_EDGE('',*,*,#3240,.F.);
#4017=ORIENTED_EDGE('',*,*,#3250,.T.);
#4018=ORIENTED_EDGE('',*,*,#3247,.T.);
#4019=ORIENTED_EDGE('',*,*,#3244,.T.);
#4020=ORIENTED_EDGE('',*,*,#3241,.T.);
#4021=ORIENTED_EDGE('',*,*,#3229,.T.);
#4022=ORIENTED_EDGE('',*,*,#3225,.T.);
#4023=ORIENTED_EDGE('',*,*,#3221,.T.);
#4024=ORIENTED_EDGE('',*,*,#3217,.T.);
#4025=ORIENTED_EDGE('',*,*,#3249,.F.);
#4026=ORIENTED_EDGE('',*,*,#3239,.F.);
#4027=ORIENTED_EDGE('',*,*,#3243,.F.);
#4028=ORIENTED_EDGE('',*,*,#3246,.F.);
#4029=ORIENTED_EDGE('',*,*,#3231,.T.);
#4030=ORIENTED_EDGE('',*,*,#3233,.T.);
#4031=ORIENTED_EDGE('',*,*,#3235,.T.);
#4032=ORIENTED_EDGE('',*,*,#3237,.T.);
#4033=ORIENTED_EDGE('',*,*,#3251,.F.);
#4034=ORIENTED_EDGE('',*,*,#3252,.T.);
#4035=ORIENTED_EDGE('',*,*,#3253,.F.);
#4036=ORIENTED_EDGE('',*,*,#3252,.F.);
#4037=ORIENTED_EDGE('',*,*,#3254,.F.);
#4038=ORIENTED_EDGE('',*,*,#3255,.T.);
#4039=ORIENTED_EDGE('',*,*,#3256,.F.);
#4040=ORIENTED_EDGE('',*,*,#3255,.F.);
#4041=ORIENTED_EDGE('',*,*,#3257,.F.);
#4042=ORIENTED_EDGE('',*,*,#3258,.T.);
#4043=ORIENTED_EDGE('',*,*,#3259,.F.);
#4044=ORIENTED_EDGE('',*,*,#3258,.F.);
#4045=ORIENTED_EDGE('',*,*,#3260,.F.);
#4046=ORIENTED_EDGE('',*,*,#3261,.T.);
#4047=ORIENTED_EDGE('',*,*,#3262,.F.);
#4048=ORIENTED_EDGE('',*,*,#3261,.F.);
#4049=ORIENTED_EDGE('',*,*,#3263,.F.);
#4050=ORIENTED_EDGE('',*,*,#3264,.T.);
#4051=ORIENTED_EDGE('',*,*,#3265,.F.);
#4052=ORIENTED_EDGE('',*,*,#3266,.F.);
#4053=ORIENTED_EDGE('',*,*,#3267,.F.);
#4054=ORIENTED_EDGE('',*,*,#3268,.F.);
#4055=ORIENTED_EDGE('',*,*,#3269,.F.);
#4056=ORIENTED_EDGE('',*,*,#3264,.F.);
#4057=ORIENTED_EDGE('',*,*,#3266,.T.);
#4058=ORIENTED_EDGE('',*,*,#3270,.F.);
#4059=ORIENTED_EDGE('',*,*,#3271,.T.);
#4060=ORIENTED_EDGE('',*,*,#3272,.T.);
#4061=ORIENTED_EDGE('',*,*,#3265,.T.);
#4062=ORIENTED_EDGE('',*,*,#3269,.T.);
#4063=ORIENTED_EDGE('',*,*,#3273,.T.);
#4064=ORIENTED_EDGE('',*,*,#3274,.T.);
#4065=ORIENTED_EDGE('',*,*,#3275,.T.);
#4066=ORIENTED_EDGE('',*,*,#3276,.T.);
#4067=ORIENTED_EDGE('',*,*,#3277,.T.);
#4068=ORIENTED_EDGE('',*,*,#3278,.T.);
#4069=ORIENTED_EDGE('',*,*,#3279,.T.);
#4070=ORIENTED_EDGE('',*,*,#3280,.T.);
#4071=ORIENTED_EDGE('',*,*,#3281,.T.);
#4072=ORIENTED_EDGE('',*,*,#3270,.T.);
#4073=ORIENTED_EDGE('',*,*,#3253,.T.);
#4074=ORIENTED_EDGE('',*,*,#3256,.T.);
#4075=ORIENTED_EDGE('',*,*,#3259,.T.);
#4076=ORIENTED_EDGE('',*,*,#3262,.T.);
#4077=ORIENTED_EDGE('',*,*,#3282,.F.);
#4078=ORIENTED_EDGE('',*,*,#3283,.T.);
#4079=ORIENTED_EDGE('',*,*,#3280,.F.);
#4080=ORIENTED_EDGE('',*,*,#3284,.F.);
#4081=ORIENTED_EDGE('',*,*,#3285,.F.);
#4082=ORIENTED_EDGE('',*,*,#3271,.F.);
#4083=ORIENTED_EDGE('',*,*,#3281,.F.);
#4084=ORIENTED_EDGE('',*,*,#3283,.F.);
#4085=ORIENTED_EDGE('',*,*,#3284,.T.);
#4086=ORIENTED_EDGE('',*,*,#3279,.F.);
#4087=ORIENTED_EDGE('',*,*,#3286,.T.);
#4088=ORIENTED_EDGE('',*,*,#3287,.T.);
#4089=ORIENTED_EDGE('',*,*,#3288,.F.);
#4090=ORIENTED_EDGE('',*,*,#3289,.T.);
#4091=ORIENTED_EDGE('',*,*,#3274,.F.);
#4092=ORIENTED_EDGE('',*,*,#3290,.F.);
#4093=ORIENTED_EDGE('',*,*,#3291,.F.);
#4094=ORIENTED_EDGE('',*,*,#3292,.F.);
#4095=ORIENTED_EDGE('',*,*,#3275,.F.);
#4096=ORIENTED_EDGE('',*,*,#3289,.F.);
#4097=ORIENTED_EDGE('',*,*,#3268,.T.);
#4098=ORIENTED_EDGE('',*,*,#3293,.T.);
#4099=ORIENTED_EDGE('',*,*,#3290,.T.);
#4100=ORIENTED_EDGE('',*,*,#3273,.F.);
#4101=ORIENTED_EDGE('',*,*,#3278,.F.);
#4102=ORIENTED_EDGE('',*,*,#3294,.F.);
#4103=ORIENTED_EDGE('',*,*,#3295,.F.);
#4104=ORIENTED_EDGE('',*,*,#3286,.F.);
#4105=ORIENTED_EDGE('',*,*,#3277,.F.);
#4106=ORIENTED_EDGE('',*,*,#3296,.F.);
#4107=ORIENTED_EDGE('',*,*,#3297,.F.);
#4108=ORIENTED_EDGE('',*,*,#3294,.T.);
#4109=ORIENTED_EDGE('',*,*,#3292,.T.);
#4110=ORIENTED_EDGE('',*,*,#3298,.T.);
#4111=ORIENTED_EDGE('',*,*,#3296,.T.);
#4112=ORIENTED_EDGE('',*,*,#3276,.F.);
#4113=ORIENTED_EDGE('',*,*,#3263,.T.);
#4114=ORIENTED_EDGE('',*,*,#3272,.F.);
#4115=ORIENTED_EDGE('',*,*,#3285,.T.);
#4116=ORIENTED_EDGE('',*,*,#3282,.T.);
#4117=ORIENTED_EDGE('',*,*,#3287,.F.);
#4118=ORIENTED_EDGE('',*,*,#3295,.T.);
#4119=ORIENTED_EDGE('',*,*,#3297,.T.);
#4120=ORIENTED_EDGE('',*,*,#3298,.F.);
#4121=ORIENTED_EDGE('',*,*,#3291,.T.);
#4122=ORIENTED_EDGE('',*,*,#3288,.T.);
#4123=ORIENTED_EDGE('',*,*,#3293,.F.);
#4124=ORIENTED_EDGE('',*,*,#3267,.T.);
#4125=ORIENTED_EDGE('',*,*,#3251,.T.);
#4126=ORIENTED_EDGE('',*,*,#3254,.T.);
#4127=ORIENTED_EDGE('',*,*,#3257,.T.);
#4128=ORIENTED_EDGE('',*,*,#3260,.T.);
#4129=ORIENTED_EDGE('',*,*,#3299,.F.);
#4130=ORIENTED_EDGE('',*,*,#3300,.T.);
#4131=ORIENTED_EDGE('',*,*,#3301,.F.);
#4132=ORIENTED_EDGE('',*,*,#3300,.F.);
#4133=ORIENTED_EDGE('',*,*,#3302,.F.);
#4134=ORIENTED_EDGE('',*,*,#3303,.T.);
#4135=ORIENTED_EDGE('',*,*,#3304,.F.);
#4136=ORIENTED_EDGE('',*,*,#3303,.F.);
#4137=ORIENTED_EDGE('',*,*,#3305,.F.);
#4138=ORIENTED_EDGE('',*,*,#3306,.T.);
#4139=ORIENTED_EDGE('',*,*,#3307,.F.);
#4140=ORIENTED_EDGE('',*,*,#3306,.F.);
#4141=ORIENTED_EDGE('',*,*,#3308,.T.);
#4142=ORIENTED_EDGE('',*,*,#3309,.T.);
#4143=ORIENTED_EDGE('',*,*,#3310,.F.);
#4144=ORIENTED_EDGE('',*,*,#3311,.F.);
#4145=ORIENTED_EDGE('',*,*,#3301,.T.);
#4146=ORIENTED_EDGE('',*,*,#3312,.T.);
#4147=ORIENTED_EDGE('',*,*,#3311,.T.);
#4148=ORIENTED_EDGE('',*,*,#3313,.F.);
#4149=ORIENTED_EDGE('',*,*,#3314,.F.);
#4150=ORIENTED_EDGE('',*,*,#3315,.T.);
#4151=ORIENTED_EDGE('',*,*,#3314,.T.);
#4152=ORIENTED_EDGE('',*,*,#3316,.F.);
#4153=ORIENTED_EDGE('',*,*,#3317,.F.);
#4154=ORIENTED_EDGE('',*,*,#3299,.T.);
#4155=ORIENTED_EDGE('',*,*,#3318,.T.);
#4156=ORIENTED_EDGE('',*,*,#3317,.T.);
#4157=ORIENTED_EDGE('',*,*,#3319,.F.);
#4158=ORIENTED_EDGE('',*,*,#3320,.F.);
#4159=ORIENTED_EDGE('',*,*,#3304,.T.);
#4160=ORIENTED_EDGE('',*,*,#3307,.T.);
#4161=ORIENTED_EDGE('',*,*,#3321,.T.);
#4162=ORIENTED_EDGE('',*,*,#3320,.T.);
#4163=ORIENTED_EDGE('',*,*,#3322,.F.);
#4164=ORIENTED_EDGE('',*,*,#3323,.F.);
#4165=ORIENTED_EDGE('',*,*,#3324,.T.);
#4166=ORIENTED_EDGE('',*,*,#3323,.T.);
#4167=ORIENTED_EDGE('',*,*,#3325,.F.);
#4168=ORIENTED_EDGE('',*,*,#3309,.F.);
#4169=ORIENTED_EDGE('',*,*,#3302,.T.);
#4170=ORIENTED_EDGE('',*,*,#3305,.T.);
#4171=ORIENTED_EDGE('',*,*,#3325,.T.);
#4172=ORIENTED_EDGE('',*,*,#3322,.T.);
#4173=ORIENTED_EDGE('',*,*,#3319,.T.);
#4174=ORIENTED_EDGE('',*,*,#3316,.T.);
#4175=ORIENTED_EDGE('',*,*,#3313,.T.);
#4176=ORIENTED_EDGE('',*,*,#3310,.T.);
#4177=ORIENTED_EDGE('',*,*,#3324,.F.);
#4178=ORIENTED_EDGE('',*,*,#3308,.F.);
#4179=ORIENTED_EDGE('',*,*,#3312,.F.);
#4180=ORIENTED_EDGE('',*,*,#3315,.F.);
#4181=ORIENTED_EDGE('',*,*,#3318,.F.);
#4182=ORIENTED_EDGE('',*,*,#3321,.F.);
#4183=ORIENTED_EDGE('',*,*,#3326,.F.);
#4184=ORIENTED_EDGE('',*,*,#3327,.T.);
#4185=ORIENTED_EDGE('',*,*,#3328,.F.);
#4186=ORIENTED_EDGE('',*,*,#3327,.F.);
#4187=ORIENTED_EDGE('',*,*,#3329,.F.);
#4188=ORIENTED_EDGE('',*,*,#3330,.T.);
#4189=ORIENTED_EDGE('',*,*,#3331,.F.);
#4190=ORIENTED_EDGE('',*,*,#3330,.F.);
#4191=ORIENTED_EDGE('',*,*,#3332,.F.);
#4192=ORIENTED_EDGE('',*,*,#3333,.T.);
#4193=ORIENTED_EDGE('',*,*,#3334,.F.);
#4194=ORIENTED_EDGE('',*,*,#3333,.F.);
#4195=ORIENTED_EDGE('',*,*,#3335,.T.);
#4196=ORIENTED_EDGE('',*,*,#3336,.T.);
#4197=ORIENTED_EDGE('',*,*,#3337,.F.);
#4198=ORIENTED_EDGE('',*,*,#3338,.F.);
#4199=ORIENTED_EDGE('',*,*,#3328,.T.);
#4200=ORIENTED_EDGE('',*,*,#3339,.T.);
#4201=ORIENTED_EDGE('',*,*,#3338,.T.);
#4202=ORIENTED_EDGE('',*,*,#3340,.F.);
#4203=ORIENTED_EDGE('',*,*,#3341,.F.);
#4204=ORIENTED_EDGE('',*,*,#3342,.T.);
#4205=ORIENTED_EDGE('',*,*,#3341,.T.);
#4206=ORIENTED_EDGE('',*,*,#3343,.F.);
#4207=ORIENTED_EDGE('',*,*,#3344,.F.);
#4208=ORIENTED_EDGE('',*,*,#3326,.T.);
#4209=ORIENTED_EDGE('',*,*,#3345,.T.);
#4210=ORIENTED_EDGE('',*,*,#3344,.T.);
#4211=ORIENTED_EDGE('',*,*,#3346,.F.);
#4212=ORIENTED_EDGE('',*,*,#3347,.F.);
#4213=ORIENTED_EDGE('',*,*,#3331,.T.);
#4214=ORIENTED_EDGE('',*,*,#3334,.T.);
#4215=ORIENTED_EDGE('',*,*,#3348,.T.);
#4216=ORIENTED_EDGE('',*,*,#3347,.T.);
#4217=ORIENTED_EDGE('',*,*,#3349,.F.);
#4218=ORIENTED_EDGE('',*,*,#3350,.F.);
#4219=ORIENTED_EDGE('',*,*,#3351,.T.);
#4220=ORIENTED_EDGE('',*,*,#3350,.T.);
#4221=ORIENTED_EDGE('',*,*,#3352,.F.);
#4222=ORIENTED_EDGE('',*,*,#3336,.F.);
#4223=ORIENTED_EDGE('',*,*,#3329,.T.);
#4224=ORIENTED_EDGE('',*,*,#3332,.T.);
#4225=ORIENTED_EDGE('',*,*,#3352,.T.);
#4226=ORIENTED_EDGE('',*,*,#3349,.T.);
#4227=ORIENTED_EDGE('',*,*,#3346,.T.);
#4228=ORIENTED_EDGE('',*,*,#3343,.T.);
#4229=ORIENTED_EDGE('',*,*,#3340,.T.);
#4230=ORIENTED_EDGE('',*,*,#3337,.T.);
#4231=ORIENTED_EDGE('',*,*,#3351,.F.);
#4232=ORIENTED_EDGE('',*,*,#3335,.F.);
#4233=ORIENTED_EDGE('',*,*,#3339,.F.);
#4234=ORIENTED_EDGE('',*,*,#3342,.F.);
#4235=ORIENTED_EDGE('',*,*,#3345,.F.);
#4236=ORIENTED_EDGE('',*,*,#3348,.F.);
#4237=ORIENTED_EDGE('',*,*,#3353,.F.);
#4238=ORIENTED_EDGE('',*,*,#3354,.T.);
#4239=ORIENTED_EDGE('',*,*,#3355,.F.);
#4240=ORIENTED_EDGE('',*,*,#3354,.F.);
#4241=ORIENTED_EDGE('',*,*,#3356,.F.);
#4242=ORIENTED_EDGE('',*,*,#3357,.T.);
#4243=ORIENTED_EDGE('',*,*,#3358,.F.);
#4244=ORIENTED_EDGE('',*,*,#3357,.F.);
#4245=ORIENTED_EDGE('',*,*,#3359,.T.);
#4246=ORIENTED_EDGE('',*,*,#3360,.T.);
#4247=ORIENTED_EDGE('',*,*,#3361,.F.);
#4248=ORIENTED_EDGE('',*,*,#3362,.F.);
#4249=ORIENTED_EDGE('',*,*,#3363,.T.);
#4250=ORIENTED_EDGE('',*,*,#3362,.T.);
#4251=ORIENTED_EDGE('',*,*,#3364,.F.);
#4252=ORIENTED_EDGE('',*,*,#3365,.F.);
#4253=ORIENTED_EDGE('',*,*,#3366,.T.);
#4254=ORIENTED_EDGE('',*,*,#3365,.T.);
#4255=ORIENTED_EDGE('',*,*,#3367,.F.);
#4256=ORIENTED_EDGE('',*,*,#3368,.F.);
#4257=ORIENTED_EDGE('',*,*,#3369,.T.);
#4258=ORIENTED_EDGE('',*,*,#3368,.T.);
#4259=ORIENTED_EDGE('',*,*,#3370,.F.);
#4260=ORIENTED_EDGE('',*,*,#3360,.F.);
#4261=ORIENTED_EDGE('',*,*,#3370,.T.);
#4262=ORIENTED_EDGE('',*,*,#3367,.T.);
#4263=ORIENTED_EDGE('',*,*,#3364,.T.);
#4264=ORIENTED_EDGE('',*,*,#3361,.T.);
#4265=ORIENTED_EDGE('',*,*,#3355,.T.);
#4266=ORIENTED_EDGE('',*,*,#3358,.T.);
#4267=ORIENTED_EDGE('',*,*,#3369,.F.);
#4268=ORIENTED_EDGE('',*,*,#3359,.F.);
#4269=ORIENTED_EDGE('',*,*,#3363,.F.);
#4270=ORIENTED_EDGE('',*,*,#3366,.F.);
#4271=ORIENTED_EDGE('',*,*,#3353,.T.);
#4272=ORIENTED_EDGE('',*,*,#3356,.T.);
#4273=ORIENTED_EDGE('',*,*,#3371,.F.);
#4274=ORIENTED_EDGE('',*,*,#3372,.T.);
#4275=ORIENTED_EDGE('',*,*,#3373,.F.);
#4276=ORIENTED_EDGE('',*,*,#3374,.F.);
#4277=ORIENTED_EDGE('',*,*,#3375,.T.);
#4278=ORIENTED_EDGE('',*,*,#3376,.F.);
#4279=ORIENTED_EDGE('',*,*,#3375,.F.);
#4280=ORIENTED_EDGE('',*,*,#3377,.F.);
#4281=ORIENTED_EDGE('',*,*,#3378,.F.);
#4282=ORIENTED_EDGE('',*,*,#3372,.F.);
#4283=ORIENTED_EDGE('',*,*,#3379,.F.);
#4284=ORIENTED_EDGE('',*,*,#3380,.F.);
#4285=ORIENTED_EDGE('',*,*,#3381,.F.);
#4286=ORIENTED_EDGE('',*,*,#3382,.T.);
#4287=ORIENTED_EDGE('',*,*,#3383,.F.);
#4288=ORIENTED_EDGE('',*,*,#3384,.F.);
#4289=ORIENTED_EDGE('',*,*,#3385,.T.);
#4290=ORIENTED_EDGE('',*,*,#3386,.F.);
#4291=ORIENTED_EDGE('',*,*,#3385,.F.);
#4292=ORIENTED_EDGE('',*,*,#3387,.F.);
#4293=ORIENTED_EDGE('',*,*,#3388,.F.);
#4294=ORIENTED_EDGE('',*,*,#3382,.F.);
#4295=ORIENTED_EDGE('',*,*,#3389,.F.);
#4296=ORIENTED_EDGE('',*,*,#3390,.F.);
#4297=ORIENTED_EDGE('',*,*,#3379,.T.);
#4298=ORIENTED_EDGE('',*,*,#3391,.T.);
#4299=ORIENTED_EDGE('',*,*,#3383,.T.);
#4300=ORIENTED_EDGE('',*,*,#3388,.T.);
#4301=ORIENTED_EDGE('',*,*,#3387,.T.);
#4302=ORIENTED_EDGE('',*,*,#3384,.T.);
#4303=ORIENTED_EDGE('',*,*,#3391,.F.);
#4304=ORIENTED_EDGE('',*,*,#3380,.T.);
#4305=ORIENTED_EDGE('',*,*,#3392,.T.);
#4306=ORIENTED_EDGE('',*,*,#3393,.T.);
#4307=ORIENTED_EDGE('',*,*,#3373,.T.);
#4308=ORIENTED_EDGE('',*,*,#3378,.T.);
#4309=ORIENTED_EDGE('',*,*,#3377,.T.);
#4310=ORIENTED_EDGE('',*,*,#3374,.T.);
#4311=ORIENTED_EDGE('',*,*,#3393,.F.);
#4312=ORIENTED_EDGE('',*,*,#3394,.T.);
#4313=ORIENTED_EDGE('',*,*,#3395,.F.);
#4314=ORIENTED_EDGE('',*,*,#3396,.T.);
#4315=ORIENTED_EDGE('',*,*,#3397,.F.);
#4316=ORIENTED_EDGE('',*,*,#3398,.T.);
#4317=ORIENTED_EDGE('',*,*,#3399,.F.);
#4318=ORIENTED_EDGE('',*,*,#3398,.F.);
#4319=ORIENTED_EDGE('',*,*,#3400,.F.);
#4320=ORIENTED_EDGE('',*,*,#3401,.F.);
#4321=ORIENTED_EDGE('',*,*,#3396,.F.);
#4322=ORIENTED_EDGE('',*,*,#3392,.F.);
#4323=ORIENTED_EDGE('',*,*,#3394,.F.);
#4324=ORIENTED_EDGE('',*,*,#3402,.F.);
#4325=ORIENTED_EDGE('',*,*,#3403,.T.);
#4326=ORIENTED_EDGE('',*,*,#3404,.F.);
#4327=ORIENTED_EDGE('',*,*,#3405,.T.);
#4328=ORIENTED_EDGE('',*,*,#3406,.F.);
#4329=ORIENTED_EDGE('',*,*,#3405,.F.);
#4330=ORIENTED_EDGE('',*,*,#3407,.F.);
#4331=ORIENTED_EDGE('',*,*,#3408,.F.);
#4332=ORIENTED_EDGE('',*,*,#3403,.F.);
#4333=ORIENTED_EDGE('',*,*,#3409,.F.);
#4334=ORIENTED_EDGE('',*,*,#3410,.F.);
#4335=ORIENTED_EDGE('',*,*,#3389,.T.);
#4336=ORIENTED_EDGE('',*,*,#3411,.T.);
#4337=ORIENTED_EDGE('',*,*,#3404,.T.);
#4338=ORIENTED_EDGE('',*,*,#3408,.T.);
#4339=ORIENTED_EDGE('',*,*,#3407,.T.);
#4340=ORIENTED_EDGE('',*,*,#3411,.F.);
#4341=ORIENTED_EDGE('',*,*,#3390,.T.);
#4342=ORIENTED_EDGE('',*,*,#3412,.F.);
#4343=ORIENTED_EDGE('',*,*,#3413,.T.);
#4344=ORIENTED_EDGE('',*,*,#3397,.T.);
#4345=ORIENTED_EDGE('',*,*,#3401,.T.);
#4346=ORIENTED_EDGE('',*,*,#3400,.T.);
#4347=ORIENTED_EDGE('',*,*,#3413,.F.);
#4348=ORIENTED_EDGE('',*,*,#3414,.F.);
#4349=ORIENTED_EDGE('',*,*,#3415,.T.);
#4350=ORIENTED_EDGE('',*,*,#3416,.F.);
#4351=ORIENTED_EDGE('',*,*,#3417,.F.);
#4352=ORIENTED_EDGE('',*,*,#3418,.F.);
#4353=ORIENTED_EDGE('',*,*,#3419,.T.);
#4354=ORIENTED_EDGE('',*,*,#3420,.F.);
#4355=ORIENTED_EDGE('',*,*,#3415,.F.);
#4356=ORIENTED_EDGE('',*,*,#3421,.F.);
#4357=ORIENTED_EDGE('',*,*,#3422,.T.);
#4358=ORIENTED_EDGE('',*,*,#3423,.F.);
#4359=ORIENTED_EDGE('',*,*,#3419,.F.);
#4360=ORIENTED_EDGE('',*,*,#3424,.F.);
#4361=ORIENTED_EDGE('',*,*,#3425,.T.);
#4362=ORIENTED_EDGE('',*,*,#3426,.F.);
#4363=ORIENTED_EDGE('',*,*,#3422,.F.);
#4364=ORIENTED_EDGE('',*,*,#3427,.F.);
#4365=ORIENTED_EDGE('',*,*,#3428,.T.);
#4366=ORIENTED_EDGE('',*,*,#3429,.F.);
#4367=ORIENTED_EDGE('',*,*,#3425,.F.);
#4368=ORIENTED_EDGE('',*,*,#3376,.T.);
#4369=ORIENTED_EDGE('',*,*,#3386,.T.);
#4370=ORIENTED_EDGE('',*,*,#3430,.F.);
#4371=ORIENTED_EDGE('',*,*,#3431,.T.);
#4372=ORIENTED_EDGE('',*,*,#3432,.F.);
#4373=ORIENTED_EDGE('',*,*,#3428,.F.);
#4374=ORIENTED_EDGE('',*,*,#3433,.F.);
#4375=ORIENTED_EDGE('',*,*,#3434,.T.);
#4376=ORIENTED_EDGE('',*,*,#3435,.F.);
#4377=ORIENTED_EDGE('',*,*,#3431,.F.);
#4378=ORIENTED_EDGE('',*,*,#3436,.F.);
#4379=ORIENTED_EDGE('',*,*,#3437,.T.);
#4380=ORIENTED_EDGE('',*,*,#3438,.F.);
#4381=ORIENTED_EDGE('',*,*,#3434,.F.);
#4382=ORIENTED_EDGE('',*,*,#3439,.F.);
#4383=ORIENTED_EDGE('',*,*,#3440,.F.);
#4384=ORIENTED_EDGE('',*,*,#3441,.F.);
#4385=ORIENTED_EDGE('',*,*,#3437,.F.);
#4386=ORIENTED_EDGE('',*,*,#3442,.F.);
#4387=ORIENTED_EDGE('',*,*,#3443,.T.);
#4388=ORIENTED_EDGE('',*,*,#3444,.F.);
#4389=ORIENTED_EDGE('',*,*,#3445,.F.);
#4390=ORIENTED_EDGE('',*,*,#3446,.F.);
#4391=ORIENTED_EDGE('',*,*,#3447,.T.);
#4392=ORIENTED_EDGE('',*,*,#3448,.F.);
#4393=ORIENTED_EDGE('',*,*,#3443,.F.);
#4394=ORIENTED_EDGE('',*,*,#3449,.F.);
#4395=ORIENTED_EDGE('',*,*,#3450,.T.);
#4396=ORIENTED_EDGE('',*,*,#3451,.F.);
#4397=ORIENTED_EDGE('',*,*,#3447,.F.);
#4398=ORIENTED_EDGE('',*,*,#3452,.F.);
#4399=ORIENTED_EDGE('',*,*,#3453,.T.);
#4400=ORIENTED_EDGE('',*,*,#3454,.F.);
#4401=ORIENTED_EDGE('',*,*,#3450,.F.);
#4402=ORIENTED_EDGE('',*,*,#3455,.F.);
#4403=ORIENTED_EDGE('',*,*,#3456,.T.);
#4404=ORIENTED_EDGE('',*,*,#3457,.F.);
#4405=ORIENTED_EDGE('',*,*,#3453,.F.);
#4406=ORIENTED_EDGE('',*,*,#3395,.T.);
#4407=ORIENTED_EDGE('',*,*,#3402,.T.);
#4408=ORIENTED_EDGE('',*,*,#3458,.F.);
#4409=ORIENTED_EDGE('',*,*,#3459,.T.);
#4410=ORIENTED_EDGE('',*,*,#3460,.F.);
#4411=ORIENTED_EDGE('',*,*,#3456,.F.);
#4412=ORIENTED_EDGE('',*,*,#3461,.F.);
#4413=ORIENTED_EDGE('',*,*,#3462,.T.);
#4414=ORIENTED_EDGE('',*,*,#3463,.F.);
#4415=ORIENTED_EDGE('',*,*,#3459,.F.);
#4416=ORIENTED_EDGE('',*,*,#3464,.F.);
#4417=ORIENTED_EDGE('',*,*,#3465,.T.);
#4418=ORIENTED_EDGE('',*,*,#3466,.F.);
#4419=ORIENTED_EDGE('',*,*,#3462,.F.);
#4420=ORIENTED_EDGE('',*,*,#3467,.F.);
#4421=ORIENTED_EDGE('',*,*,#3468,.F.);
#4422=ORIENTED_EDGE('',*,*,#3469,.F.);
#4423=ORIENTED_EDGE('',*,*,#3465,.F.);
#4424=ORIENTED_EDGE('',*,*,#3470,.F.);
#4425=ORIENTED_EDGE('',*,*,#3471,.T.);
#4426=ORIENTED_EDGE('',*,*,#3472,.F.);
#4427=ORIENTED_EDGE('',*,*,#3473,.F.);
#4428=ORIENTED_EDGE('',*,*,#3474,.F.);
#4429=ORIENTED_EDGE('',*,*,#3475,.T.);
#4430=ORIENTED_EDGE('',*,*,#3476,.F.);
#4431=ORIENTED_EDGE('',*,*,#3471,.F.);
#4432=ORIENTED_EDGE('',*,*,#3477,.F.);
#4433=ORIENTED_EDGE('',*,*,#3478,.T.);
#4434=ORIENTED_EDGE('',*,*,#3479,.F.);
#4435=ORIENTED_EDGE('',*,*,#3475,.F.);
#4436=ORIENTED_EDGE('',*,*,#3480,.F.);
#4437=ORIENTED_EDGE('',*,*,#3481,.T.);
#4438=ORIENTED_EDGE('',*,*,#3482,.F.);
#4439=ORIENTED_EDGE('',*,*,#3478,.F.);
#4440=ORIENTED_EDGE('',*,*,#3483,.F.);
#4441=ORIENTED_EDGE('',*,*,#3484,.T.);
#4442=ORIENTED_EDGE('',*,*,#3485,.F.);
#4443=ORIENTED_EDGE('',*,*,#3481,.F.);
#4444=ORIENTED_EDGE('',*,*,#3371,.T.);
#4445=ORIENTED_EDGE('',*,*,#3381,.T.);
#4446=ORIENTED_EDGE('',*,*,#3486,.F.);
#4447=ORIENTED_EDGE('',*,*,#3487,.T.);
#4448=ORIENTED_EDGE('',*,*,#3488,.F.);
#4449=ORIENTED_EDGE('',*,*,#3484,.F.);
#4450=ORIENTED_EDGE('',*,*,#3489,.F.);
#4451=ORIENTED_EDGE('',*,*,#3490,.T.);
#4452=ORIENTED_EDGE('',*,*,#3491,.F.);
#4453=ORIENTED_EDGE('',*,*,#3487,.F.);
#4454=ORIENTED_EDGE('',*,*,#3492,.F.);
#4455=ORIENTED_EDGE('',*,*,#3493,.T.);
#4456=ORIENTED_EDGE('',*,*,#3494,.F.);
#4457=ORIENTED_EDGE('',*,*,#3490,.F.);
#4458=ORIENTED_EDGE('',*,*,#3495,.F.);
#4459=ORIENTED_EDGE('',*,*,#3496,.F.);
#4460=ORIENTED_EDGE('',*,*,#3497,.F.);
#4461=ORIENTED_EDGE('',*,*,#3493,.F.);
#4462=ORIENTED_EDGE('',*,*,#3498,.F.);
#4463=ORIENTED_EDGE('',*,*,#3499,.T.);
#4464=ORIENTED_EDGE('',*,*,#3500,.F.);
#4465=ORIENTED_EDGE('',*,*,#3501,.F.);
#4466=ORIENTED_EDGE('',*,*,#3502,.F.);
#4467=ORIENTED_EDGE('',*,*,#3503,.T.);
#4468=ORIENTED_EDGE('',*,*,#3504,.F.);
#4469=ORIENTED_EDGE('',*,*,#3499,.F.);
#4470=ORIENTED_EDGE('',*,*,#3505,.F.);
#4471=ORIENTED_EDGE('',*,*,#3506,.T.);
#4472=ORIENTED_EDGE('',*,*,#3507,.F.);
#4473=ORIENTED_EDGE('',*,*,#3503,.F.);
#4474=ORIENTED_EDGE('',*,*,#3508,.F.);
#4475=ORIENTED_EDGE('',*,*,#3509,.T.);
#4476=ORIENTED_EDGE('',*,*,#3510,.F.);
#4477=ORIENTED_EDGE('',*,*,#3506,.F.);
#4478=ORIENTED_EDGE('',*,*,#3511,.F.);
#4479=ORIENTED_EDGE('',*,*,#3512,.T.);
#4480=ORIENTED_EDGE('',*,*,#3513,.F.);
#4481=ORIENTED_EDGE('',*,*,#3509,.F.);
#4482=ORIENTED_EDGE('',*,*,#3399,.T.);
#4483=ORIENTED_EDGE('',*,*,#3406,.T.);
#4484=ORIENTED_EDGE('',*,*,#3514,.F.);
#4485=ORIENTED_EDGE('',*,*,#3515,.T.);
#4486=ORIENTED_EDGE('',*,*,#3516,.F.);
#4487=ORIENTED_EDGE('',*,*,#3512,.F.);
#4488=ORIENTED_EDGE('',*,*,#3517,.F.);
#4489=ORIENTED_EDGE('',*,*,#3518,.T.);
#4490=ORIENTED_EDGE('',*,*,#3519,.F.);
#4491=ORIENTED_EDGE('',*,*,#3515,.F.);
#4492=ORIENTED_EDGE('',*,*,#3520,.F.);
#4493=ORIENTED_EDGE('',*,*,#3521,.T.);
#4494=ORIENTED_EDGE('',*,*,#3522,.F.);
#4495=ORIENTED_EDGE('',*,*,#3518,.F.);
#4496=ORIENTED_EDGE('',*,*,#3523,.F.);
#4497=ORIENTED_EDGE('',*,*,#3524,.F.);
#4498=ORIENTED_EDGE('',*,*,#3525,.F.);
#4499=ORIENTED_EDGE('',*,*,#3521,.F.);
#4500=ORIENTED_EDGE('',*,*,#3409,.T.);
#4501=ORIENTED_EDGE('',*,*,#3526,.T.);
#4502=ORIENTED_EDGE('',*,*,#3527,.F.);
#4503=ORIENTED_EDGE('',*,*,#3526,.F.);
#4504=ORIENTED_EDGE('',*,*,#3410,.T.);
#4505=ORIENTED_EDGE('',*,*,#3440,.T.);
#4506=ORIENTED_EDGE('',*,*,#3528,.T.);
#4507=ORIENTED_EDGE('',*,*,#3529,.T.);
#4508=ORIENTED_EDGE('',*,*,#3530,.F.);
#4509=ORIENTED_EDGE('',*,*,#3417,.T.);
#4510=ORIENTED_EDGE('',*,*,#3531,.F.);
#4511=ORIENTED_EDGE('',*,*,#3532,.F.);
#4512=ORIENTED_EDGE('',*,*,#3533,.T.);
#4513=ORIENTED_EDGE('',*,*,#3468,.T.);
#4514=ORIENTED_EDGE('',*,*,#3534,.T.);
#4515=ORIENTED_EDGE('',*,*,#3532,.T.);
#4516=ORIENTED_EDGE('',*,*,#3535,.F.);
#4517=ORIENTED_EDGE('',*,*,#3445,.T.);
#4518=ORIENTED_EDGE('',*,*,#3536,.F.);
#4519=ORIENTED_EDGE('',*,*,#3537,.F.);
#4520=ORIENTED_EDGE('',*,*,#3538,.T.);
#4521=ORIENTED_EDGE('',*,*,#3496,.T.);
#4522=ORIENTED_EDGE('',*,*,#3539,.T.);
#4523=ORIENTED_EDGE('',*,*,#3537,.T.);
#4524=ORIENTED_EDGE('',*,*,#3540,.F.);
#4525=ORIENTED_EDGE('',*,*,#3473,.T.);
#4526=ORIENTED_EDGE('',*,*,#3541,.F.);
#4527=ORIENTED_EDGE('',*,*,#3542,.F.);
#4528=ORIENTED_EDGE('',*,*,#3543,.T.);
#4529=ORIENTED_EDGE('',*,*,#3524,.T.);
#4530=ORIENTED_EDGE('',*,*,#3544,.T.);
#4531=ORIENTED_EDGE('',*,*,#3542,.T.);
#4532=ORIENTED_EDGE('',*,*,#3545,.F.);
#4533=ORIENTED_EDGE('',*,*,#3501,.T.);
#4534=ORIENTED_EDGE('',*,*,#3546,.F.);
#4535=ORIENTED_EDGE('',*,*,#3529,.F.);
#4536=ORIENTED_EDGE('',*,*,#3547,.T.);
#4537=ORIENTED_EDGE('',*,*,#3416,.T.);
#4538=ORIENTED_EDGE('',*,*,#3420,.T.);
#4539=ORIENTED_EDGE('',*,*,#3423,.T.);
#4540=ORIENTED_EDGE('',*,*,#3426,.T.);
#4541=ORIENTED_EDGE('',*,*,#3429,.T.);
#4542=ORIENTED_EDGE('',*,*,#3432,.T.);
#4543=ORIENTED_EDGE('',*,*,#3435,.T.);
#4544=ORIENTED_EDGE('',*,*,#3438,.T.);
#4545=ORIENTED_EDGE('',*,*,#3441,.T.);
#4546=ORIENTED_EDGE('',*,*,#3530,.T.);
#4547=ORIENTED_EDGE('',*,*,#3546,.T.);
#4548=ORIENTED_EDGE('',*,*,#3500,.T.);
#4549=ORIENTED_EDGE('',*,*,#3504,.T.);
#4550=ORIENTED_EDGE('',*,*,#3507,.T.);
#4551=ORIENTED_EDGE('',*,*,#3510,.T.);
#4552=ORIENTED_EDGE('',*,*,#3513,.T.);
#4553=ORIENTED_EDGE('',*,*,#3516,.T.);
#4554=ORIENTED_EDGE('',*,*,#3519,.T.);
#4555=ORIENTED_EDGE('',*,*,#3522,.T.);
#4556=ORIENTED_EDGE('',*,*,#3525,.T.);
#4557=ORIENTED_EDGE('',*,*,#3545,.T.);
#4558=ORIENTED_EDGE('',*,*,#3541,.T.);
#4559=ORIENTED_EDGE('',*,*,#3472,.T.);
#4560=ORIENTED_EDGE('',*,*,#3476,.T.);
#4561=ORIENTED_EDGE('',*,*,#3479,.T.);
#4562=ORIENTED_EDGE('',*,*,#3482,.T.);
#4563=ORIENTED_EDGE('',*,*,#3485,.T.);
#4564=ORIENTED_EDGE('',*,*,#3488,.T.);
#4565=ORIENTED_EDGE('',*,*,#3491,.T.);
#4566=ORIENTED_EDGE('',*,*,#3494,.T.);
#4567=ORIENTED_EDGE('',*,*,#3497,.T.);
#4568=ORIENTED_EDGE('',*,*,#3540,.T.);
#4569=ORIENTED_EDGE('',*,*,#3536,.T.);
#4570=ORIENTED_EDGE('',*,*,#3444,.T.);
#4571=ORIENTED_EDGE('',*,*,#3448,.T.);
#4572=ORIENTED_EDGE('',*,*,#3451,.T.);
#4573=ORIENTED_EDGE('',*,*,#3454,.T.);
#4574=ORIENTED_EDGE('',*,*,#3457,.T.);
#4575=ORIENTED_EDGE('',*,*,#3460,.T.);
#4576=ORIENTED_EDGE('',*,*,#3463,.T.);
#4577=ORIENTED_EDGE('',*,*,#3466,.T.);
#4578=ORIENTED_EDGE('',*,*,#3469,.T.);
#4579=ORIENTED_EDGE('',*,*,#3535,.T.);
#4580=ORIENTED_EDGE('',*,*,#3531,.T.);
#4581=ORIENTED_EDGE('',*,*,#3527,.T.);
#4582=ORIENTED_EDGE('',*,*,#3414,.T.);
#4583=ORIENTED_EDGE('',*,*,#3533,.F.);
#4584=ORIENTED_EDGE('',*,*,#3534,.F.);
#4585=ORIENTED_EDGE('',*,*,#3467,.T.);
#4586=ORIENTED_EDGE('',*,*,#3464,.T.);
#4587=ORIENTED_EDGE('',*,*,#3461,.T.);
#4588=ORIENTED_EDGE('',*,*,#3458,.T.);
#4589=ORIENTED_EDGE('',*,*,#3455,.T.);
#4590=ORIENTED_EDGE('',*,*,#3452,.T.);
#4591=ORIENTED_EDGE('',*,*,#3449,.T.);
#4592=ORIENTED_EDGE('',*,*,#3446,.T.);
#4593=ORIENTED_EDGE('',*,*,#3442,.T.);
#4594=ORIENTED_EDGE('',*,*,#3538,.F.);
#4595=ORIENTED_EDGE('',*,*,#3539,.F.);
#4596=ORIENTED_EDGE('',*,*,#3495,.T.);
#4597=ORIENTED_EDGE('',*,*,#3492,.T.);
#4598=ORIENTED_EDGE('',*,*,#3489,.T.);
#4599=ORIENTED_EDGE('',*,*,#3486,.T.);
#4600=ORIENTED_EDGE('',*,*,#3483,.T.);
#4601=ORIENTED_EDGE('',*,*,#3480,.T.);
#4602=ORIENTED_EDGE('',*,*,#3477,.T.);
#4603=ORIENTED_EDGE('',*,*,#3474,.T.);
#4604=ORIENTED_EDGE('',*,*,#3470,.T.);
#4605=ORIENTED_EDGE('',*,*,#3543,.F.);
#4606=ORIENTED_EDGE('',*,*,#3544,.F.);
#4607=ORIENTED_EDGE('',*,*,#3523,.T.);
#4608=ORIENTED_EDGE('',*,*,#3520,.T.);
#4609=ORIENTED_EDGE('',*,*,#3517,.T.);
#4610=ORIENTED_EDGE('',*,*,#3514,.T.);
#4611=ORIENTED_EDGE('',*,*,#3511,.T.);
#4612=ORIENTED_EDGE('',*,*,#3508,.T.);
#4613=ORIENTED_EDGE('',*,*,#3505,.T.);
#4614=ORIENTED_EDGE('',*,*,#3502,.T.);
#4615=ORIENTED_EDGE('',*,*,#3498,.T.);
#4616=ORIENTED_EDGE('',*,*,#3547,.F.);
#4617=ORIENTED_EDGE('',*,*,#3528,.F.);
#4618=ORIENTED_EDGE('',*,*,#3439,.T.);
#4619=ORIENTED_EDGE('',*,*,#3436,.T.);
#4620=ORIENTED_EDGE('',*,*,#3433,.T.);
#4621=ORIENTED_EDGE('',*,*,#3430,.T.);
#4622=ORIENTED_EDGE('',*,*,#3427,.T.);
#4623=ORIENTED_EDGE('',*,*,#3424,.T.);
#4624=ORIENTED_EDGE('',*,*,#3421,.T.);
#4625=ORIENTED_EDGE('',*,*,#3418,.T.);
#4626=ORIENTED_EDGE('',*,*,#3412,.T.);
#4627=ORIENTED_EDGE('',*,*,#3548,.F.);
#4628=ORIENTED_EDGE('',*,*,#3549,.F.);
#4629=ORIENTED_EDGE('',*,*,#3550,.F.);
#4630=ORIENTED_EDGE('',*,*,#3551,.F.);
#4631=ORIENTED_EDGE('',*,*,#3552,.F.);
#4632=ORIENTED_EDGE('',*,*,#3553,.F.);
#4633=ORIENTED_EDGE('',*,*,#3554,.F.);
#4634=ORIENTED_EDGE('',*,*,#3555,.F.);
#4635=ORIENTED_EDGE('',*,*,#3556,.F.);
#4636=ORIENTED_EDGE('',*,*,#3557,.F.);
#4637=ORIENTED_EDGE('',*,*,#3558,.F.);
#4638=ORIENTED_EDGE('',*,*,#3559,.F.);
#4639=ORIENTED_EDGE('',*,*,#3560,.F.);
#4640=ORIENTED_EDGE('',*,*,#3561,.F.);
#4641=ORIENTED_EDGE('',*,*,#3562,.F.);
#4642=ORIENTED_EDGE('',*,*,#3563,.F.);
#4643=ORIENTED_EDGE('',*,*,#3564,.F.);
#4644=ORIENTED_EDGE('',*,*,#3565,.F.);
#4645=ORIENTED_EDGE('',*,*,#3566,.F.);
#4646=ORIENTED_EDGE('',*,*,#3567,.F.);
#4647=ORIENTED_EDGE('',*,*,#3568,.F.);
#4648=ORIENTED_EDGE('',*,*,#3569,.F.);
#4649=ORIENTED_EDGE('',*,*,#3570,.F.);
#4650=ORIENTED_EDGE('',*,*,#3571,.F.);
#4651=ORIENTED_EDGE('',*,*,#3572,.F.);
#4652=ORIENTED_EDGE('',*,*,#3573,.F.);
#4653=ORIENTED_EDGE('',*,*,#3574,.F.);
#4654=ORIENTED_EDGE('',*,*,#3575,.F.);
#4655=ORIENTED_EDGE('',*,*,#3576,.F.);
#4656=ORIENTED_EDGE('',*,*,#3577,.F.);
#4657=ORIENTED_EDGE('',*,*,#3578,.F.);
#4658=ORIENTED_EDGE('',*,*,#3579,.F.);
#4659=ORIENTED_EDGE('',*,*,#3580,.F.);
#4660=ORIENTED_EDGE('',*,*,#3581,.F.);
#4661=ORIENTED_EDGE('',*,*,#3582,.F.);
#4662=ORIENTED_EDGE('',*,*,#3583,.F.);
#4663=ORIENTED_EDGE('',*,*,#3584,.F.);
#4664=ORIENTED_EDGE('',*,*,#3585,.F.);
#4665=ORIENTED_EDGE('',*,*,#3586,.F.);
#4666=ORIENTED_EDGE('',*,*,#3587,.F.);
#4667=ORIENTED_EDGE('',*,*,#3588,.F.);
#4668=ORIENTED_EDGE('',*,*,#3589,.F.);
#4669=ORIENTED_EDGE('',*,*,#3590,.F.);
#4670=ORIENTED_EDGE('',*,*,#3591,.F.);
#4671=ORIENTED_EDGE('',*,*,#3592,.F.);
#4672=ORIENTED_EDGE('',*,*,#3570,.T.);
#4673=ORIENTED_EDGE('',*,*,#3593,.F.);
#4674=ORIENTED_EDGE('',*,*,#3594,.F.);
#4675=ORIENTED_EDGE('',*,*,#3595,.T.);
#4676=ORIENTED_EDGE('',*,*,#3569,.T.);
#4677=ORIENTED_EDGE('',*,*,#3596,.F.);
#4678=ORIENTED_EDGE('',*,*,#3597,.T.);
#4679=ORIENTED_EDGE('',*,*,#3593,.T.);
#4680=ORIENTED_EDGE('',*,*,#3568,.T.);
#4681=ORIENTED_EDGE('',*,*,#3598,.T.);
#4682=ORIENTED_EDGE('',*,*,#3599,.T.);
#4683=ORIENTED_EDGE('',*,*,#3596,.T.);
#4684=ORIENTED_EDGE('',*,*,#3567,.T.);
#4685=ORIENTED_EDGE('',*,*,#3600,.F.);
#4686=ORIENTED_EDGE('',*,*,#3601,.F.);
#4687=ORIENTED_EDGE('',*,*,#3598,.F.);
#4688=ORIENTED_EDGE('',*,*,#3566,.T.);
#4689=ORIENTED_EDGE('',*,*,#3602,.F.);
#4690=ORIENTED_EDGE('',*,*,#3603,.F.);
#4691=ORIENTED_EDGE('',*,*,#3600,.T.);
#4692=ORIENTED_EDGE('',*,*,#3565,.T.);
#4693=ORIENTED_EDGE('',*,*,#3604,.F.);
#4694=ORIENTED_EDGE('',*,*,#3605,.F.);
#4695=ORIENTED_EDGE('',*,*,#3602,.T.);
#4696=ORIENTED_EDGE('',*,*,#3564,.T.);
#4697=ORIENTED_EDGE('',*,*,#3606,.F.);
#4698=ORIENTED_EDGE('',*,*,#3607,.F.);
#4699=ORIENTED_EDGE('',*,*,#3604,.T.);
#4700=ORIENTED_EDGE('',*,*,#3563,.T.);
#4701=ORIENTED_EDGE('',*,*,#3608,.F.);
#4702=ORIENTED_EDGE('',*,*,#3609,.F.);
#4703=ORIENTED_EDGE('',*,*,#3606,.T.);
#4704=ORIENTED_EDGE('',*,*,#3562,.T.);
#4705=ORIENTED_EDGE('',*,*,#3610,.F.);
#4706=ORIENTED_EDGE('',*,*,#3611,.F.);
#4707=ORIENTED_EDGE('',*,*,#3608,.T.);
#4708=ORIENTED_EDGE('',*,*,#3561,.T.);
#4709=ORIENTED_EDGE('',*,*,#3612,.F.);
#4710=ORIENTED_EDGE('',*,*,#3613,.F.);
#4711=ORIENTED_EDGE('',*,*,#3610,.T.);
#4712=ORIENTED_EDGE('',*,*,#3560,.T.);
#4713=ORIENTED_EDGE('',*,*,#3614,.F.);
#4714=ORIENTED_EDGE('',*,*,#3615,.F.);
#4715=ORIENTED_EDGE('',*,*,#3612,.T.);
#4716=ORIENTED_EDGE('',*,*,#3559,.T.);
#4717=ORIENTED_EDGE('',*,*,#3616,.F.);
#4718=ORIENTED_EDGE('',*,*,#3617,.F.);
#4719=ORIENTED_EDGE('',*,*,#3614,.T.);
#4720=ORIENTED_EDGE('',*,*,#3558,.T.);
#4721=ORIENTED_EDGE('',*,*,#3618,.F.);
#4722=ORIENTED_EDGE('',*,*,#3619,.T.);
#4723=ORIENTED_EDGE('',*,*,#3616,.T.);
#4724=ORIENTED_EDGE('',*,*,#3557,.T.);
#4725=ORIENTED_EDGE('',*,*,#3620,.T.);
#4726=ORIENTED_EDGE('',*,*,#3621,.T.);
#4727=ORIENTED_EDGE('',*,*,#3618,.T.);
#4728=ORIENTED_EDGE('',*,*,#3556,.T.);
#4729=ORIENTED_EDGE('',*,*,#3622,.F.);
#4730=ORIENTED_EDGE('',*,*,#3623,.F.);
#4731=ORIENTED_EDGE('',*,*,#3620,.F.);
#4732=ORIENTED_EDGE('',*,*,#3555,.T.);
#4733=ORIENTED_EDGE('',*,*,#3624,.F.);
#4734=ORIENTED_EDGE('',*,*,#3625,.F.);
#4735=ORIENTED_EDGE('',*,*,#3622,.T.);
#4736=ORIENTED_EDGE('',*,*,#3554,.T.);
#4737=ORIENTED_EDGE('',*,*,#3626,.F.);
#4738=ORIENTED_EDGE('',*,*,#3627,.F.);
#4739=ORIENTED_EDGE('',*,*,#3624,.T.);
#4740=ORIENTED_EDGE('',*,*,#3553,.T.);
#4741=ORIENTED_EDGE('',*,*,#3628,.F.);
#4742=ORIENTED_EDGE('',*,*,#3629,.F.);
#4743=ORIENTED_EDGE('',*,*,#3626,.T.);
#4744=ORIENTED_EDGE('',*,*,#3552,.T.);
#4745=ORIENTED_EDGE('',*,*,#3630,.F.);
#4746=ORIENTED_EDGE('',*,*,#3631,.F.);
#4747=ORIENTED_EDGE('',*,*,#3628,.T.);
#4748=ORIENTED_EDGE('',*,*,#3551,.T.);
#4749=ORIENTED_EDGE('',*,*,#3632,.F.);
#4750=ORIENTED_EDGE('',*,*,#3633,.F.);
#4751=ORIENTED_EDGE('',*,*,#3630,.T.);
#4752=ORIENTED_EDGE('',*,*,#3550,.T.);
#4753=ORIENTED_EDGE('',*,*,#3634,.F.);
#4754=ORIENTED_EDGE('',*,*,#3635,.F.);
#4755=ORIENTED_EDGE('',*,*,#3632,.T.);
#4756=ORIENTED_EDGE('',*,*,#3549,.T.);
#4757=ORIENTED_EDGE('',*,*,#3636,.F.);
#4758=ORIENTED_EDGE('',*,*,#3637,.F.);
#4759=ORIENTED_EDGE('',*,*,#3634,.T.);
#4760=ORIENTED_EDGE('',*,*,#3581,.T.);
#4761=ORIENTED_EDGE('',*,*,#3638,.F.);
#4762=ORIENTED_EDGE('',*,*,#3639,.F.);
#4763=ORIENTED_EDGE('',*,*,#3640,.T.);
#4764=ORIENTED_EDGE('',*,*,#3582,.T.);
#4765=ORIENTED_EDGE('',*,*,#3640,.F.);
#4766=ORIENTED_EDGE('',*,*,#3641,.F.);
#4767=ORIENTED_EDGE('',*,*,#3642,.T.);
#4768=ORIENTED_EDGE('',*,*,#3583,.T.);
#4769=ORIENTED_EDGE('',*,*,#3642,.F.);
#4770=ORIENTED_EDGE('',*,*,#3643,.F.);
#4771=ORIENTED_EDGE('',*,*,#3644,.T.);
#4772=ORIENTED_EDGE('',*,*,#3584,.T.);
#4773=ORIENTED_EDGE('',*,*,#3644,.F.);
#4774=ORIENTED_EDGE('',*,*,#3645,.F.);
#4775=ORIENTED_EDGE('',*,*,#3646,.T.);
#4776=ORIENTED_EDGE('',*,*,#3585,.T.);
#4777=ORIENTED_EDGE('',*,*,#3646,.F.);
#4778=ORIENTED_EDGE('',*,*,#3647,.F.);
#4779=ORIENTED_EDGE('',*,*,#3648,.T.);
#4780=ORIENTED_EDGE('',*,*,#3586,.T.);
#4781=ORIENTED_EDGE('',*,*,#3648,.F.);
#4782=ORIENTED_EDGE('',*,*,#3649,.F.);
#4783=ORIENTED_EDGE('',*,*,#3650,.T.);
#4784=ORIENTED_EDGE('',*,*,#3587,.T.);
#4785=ORIENTED_EDGE('',*,*,#3650,.F.);
#4786=ORIENTED_EDGE('',*,*,#3651,.F.);
#4787=ORIENTED_EDGE('',*,*,#3652,.T.);
#4788=ORIENTED_EDGE('',*,*,#3588,.T.);
#4789=ORIENTED_EDGE('',*,*,#3652,.F.);
#4790=ORIENTED_EDGE('',*,*,#3653,.F.);
#4791=ORIENTED_EDGE('',*,*,#3654,.T.);
#4792=ORIENTED_EDGE('',*,*,#3589,.T.);
#4793=ORIENTED_EDGE('',*,*,#3654,.F.);
#4794=ORIENTED_EDGE('',*,*,#3655,.F.);
#4795=ORIENTED_EDGE('',*,*,#3656,.F.);
#4796=ORIENTED_EDGE('',*,*,#3571,.T.);
#4797=ORIENTED_EDGE('',*,*,#3595,.F.);
#4798=ORIENTED_EDGE('',*,*,#3657,.F.);
#4799=ORIENTED_EDGE('',*,*,#3658,.T.);
#4800=ORIENTED_EDGE('',*,*,#3572,.T.);
#4801=ORIENTED_EDGE('',*,*,#3658,.F.);
#4802=ORIENTED_EDGE('',*,*,#3659,.F.);
#4803=ORIENTED_EDGE('',*,*,#3660,.T.);
#4804=ORIENTED_EDGE('',*,*,#3573,.T.);
#4805=ORIENTED_EDGE('',*,*,#3660,.F.);
#4806=ORIENTED_EDGE('',*,*,#3661,.F.);
#4807=ORIENTED_EDGE('',*,*,#3662,.T.);
#4808=ORIENTED_EDGE('',*,*,#3574,.T.);
#4809=ORIENTED_EDGE('',*,*,#3662,.F.);
#4810=ORIENTED_EDGE('',*,*,#3663,.F.);
#4811=ORIENTED_EDGE('',*,*,#3664,.T.);
#4812=ORIENTED_EDGE('',*,*,#3575,.T.);
#4813=ORIENTED_EDGE('',*,*,#3664,.F.);
#4814=ORIENTED_EDGE('',*,*,#3665,.F.);
#4815=ORIENTED_EDGE('',*,*,#3666,.T.);
#4816=ORIENTED_EDGE('',*,*,#3576,.T.);
#4817=ORIENTED_EDGE('',*,*,#3666,.F.);
#4818=ORIENTED_EDGE('',*,*,#3667,.F.);
#4819=ORIENTED_EDGE('',*,*,#3668,.T.);
#4820=ORIENTED_EDGE('',*,*,#3577,.T.);
#4821=ORIENTED_EDGE('',*,*,#3668,.F.);
#4822=ORIENTED_EDGE('',*,*,#3669,.F.);
#4823=ORIENTED_EDGE('',*,*,#3670,.T.);
#4824=ORIENTED_EDGE('',*,*,#3578,.T.);
#4825=ORIENTED_EDGE('',*,*,#3670,.F.);
#4826=ORIENTED_EDGE('',*,*,#3671,.F.);
#4827=ORIENTED_EDGE('',*,*,#3672,.F.);
#4828=ORIENTED_EDGE('',*,*,#3548,.T.);
#4829=ORIENTED_EDGE('',*,*,#3673,.F.);
#4830=ORIENTED_EDGE('',*,*,#3674,.F.);
#4831=ORIENTED_EDGE('',*,*,#3636,.T.);
#4832=ORIENTED_EDGE('',*,*,#3675,.F.);
#4833=ORIENTED_EDGE('',*,*,#3676,.T.);
#4834=ORIENTED_EDGE('',*,*,#3592,.T.);
#4835=ORIENTED_EDGE('',*,*,#3676,.F.);
#4836=ORIENTED_EDGE('',*,*,#3590,.T.);
#4837=ORIENTED_EDGE('',*,*,#3656,.T.);
#4838=ORIENTED_EDGE('',*,*,#3677,.T.);
#4839=ORIENTED_EDGE('',*,*,#3678,.T.);
#4840=ORIENTED_EDGE('',*,*,#3580,.T.);
#4841=ORIENTED_EDGE('',*,*,#3679,.F.);
#4842=ORIENTED_EDGE('',*,*,#3680,.T.);
#4843=ORIENTED_EDGE('',*,*,#3638,.T.);
#4844=ORIENTED_EDGE('',*,*,#3579,.T.);
#4845=ORIENTED_EDGE('',*,*,#3672,.T.);
#4846=ORIENTED_EDGE('',*,*,#3681,.T.);
#4847=ORIENTED_EDGE('',*,*,#3679,.T.);
#4848=ORIENTED_EDGE('',*,*,#3591,.T.);
#4849=ORIENTED_EDGE('',*,*,#3678,.F.);
#4850=ORIENTED_EDGE('',*,*,#3682,.T.);
#4851=ORIENTED_EDGE('',*,*,#3673,.T.);
#4852=ORIENTED_EDGE('',*,*,#3639,.T.);
#4853=ORIENTED_EDGE('',*,*,#3680,.F.);
#4854=ORIENTED_EDGE('',*,*,#3681,.F.);
#4855=ORIENTED_EDGE('',*,*,#3671,.T.);
#4856=ORIENTED_EDGE('',*,*,#3669,.T.);
#4857=ORIENTED_EDGE('',*,*,#3667,.T.);
#4858=ORIENTED_EDGE('',*,*,#3665,.T.);
#4859=ORIENTED_EDGE('',*,*,#3663,.T.);
#4860=ORIENTED_EDGE('',*,*,#3661,.T.);
#4861=ORIENTED_EDGE('',*,*,#3659,.T.);
#4862=ORIENTED_EDGE('',*,*,#3657,.T.);
#4863=ORIENTED_EDGE('',*,*,#3594,.T.);
#4864=ORIENTED_EDGE('',*,*,#3597,.F.);
#4865=ORIENTED_EDGE('',*,*,#3599,.F.);
#4866=ORIENTED_EDGE('',*,*,#3601,.T.);
#4867=ORIENTED_EDGE('',*,*,#3603,.T.);
#4868=ORIENTED_EDGE('',*,*,#3605,.T.);
#4869=ORIENTED_EDGE('',*,*,#3607,.T.);
#4870=ORIENTED_EDGE('',*,*,#3609,.T.);
#4871=ORIENTED_EDGE('',*,*,#3611,.T.);
#4872=ORIENTED_EDGE('',*,*,#3613,.T.);
#4873=ORIENTED_EDGE('',*,*,#3615,.T.);
#4874=ORIENTED_EDGE('',*,*,#3617,.T.);
#4875=ORIENTED_EDGE('',*,*,#3619,.F.);
#4876=ORIENTED_EDGE('',*,*,#3621,.F.);
#4877=ORIENTED_EDGE('',*,*,#3623,.T.);
#4878=ORIENTED_EDGE('',*,*,#3625,.T.);
#4879=ORIENTED_EDGE('',*,*,#3627,.T.);
#4880=ORIENTED_EDGE('',*,*,#3629,.T.);
#4881=ORIENTED_EDGE('',*,*,#3631,.T.);
#4882=ORIENTED_EDGE('',*,*,#3633,.T.);
#4883=ORIENTED_EDGE('',*,*,#3635,.T.);
#4884=ORIENTED_EDGE('',*,*,#3637,.T.);
#4885=ORIENTED_EDGE('',*,*,#3674,.T.);
#4886=ORIENTED_EDGE('',*,*,#3682,.F.);
#4887=ORIENTED_EDGE('',*,*,#3677,.F.);
#4888=ORIENTED_EDGE('',*,*,#3655,.T.);
#4889=ORIENTED_EDGE('',*,*,#3653,.T.);
#4890=ORIENTED_EDGE('',*,*,#3651,.T.);
#4891=ORIENTED_EDGE('',*,*,#3649,.T.);
#4892=ORIENTED_EDGE('',*,*,#3647,.T.);
#4893=ORIENTED_EDGE('',*,*,#3645,.T.);
#4894=ORIENTED_EDGE('',*,*,#3643,.T.);
#4895=ORIENTED_EDGE('',*,*,#3641,.T.);
#4896=ORIENTED_EDGE('',*,*,#3675,.T.);
#4897=ORIENTED_EDGE('',*,*,#3683,.T.);
#4898=ORIENTED_EDGE('',*,*,#3684,.T.);
#4899=ORIENTED_EDGE('',*,*,#3685,.T.);
#4900=ORIENTED_EDGE('',*,*,#3686,.F.);
#4901=ORIENTED_EDGE('',*,*,#3687,.T.);
#4902=ORIENTED_EDGE('',*,*,#3688,.T.);
#4903=ORIENTED_EDGE('',*,*,#3689,.T.);
#4904=ORIENTED_EDGE('',*,*,#3684,.F.);
#4905=ORIENTED_EDGE('',*,*,#3690,.T.);
#4906=ORIENTED_EDGE('',*,*,#3691,.T.);
#4907=ORIENTED_EDGE('',*,*,#3692,.T.);
#4908=ORIENTED_EDGE('',*,*,#3688,.F.);
#4909=ORIENTED_EDGE('',*,*,#3693,.T.);
#4910=ORIENTED_EDGE('',*,*,#3694,.T.);
#4911=ORIENTED_EDGE('',*,*,#3695,.T.);
#4912=ORIENTED_EDGE('',*,*,#3691,.F.);
#4913=ORIENTED_EDGE('',*,*,#3696,.T.);
#4914=ORIENTED_EDGE('',*,*,#3697,.T.);
#4915=ORIENTED_EDGE('',*,*,#3698,.T.);
#4916=ORIENTED_EDGE('',*,*,#3694,.F.);
#4917=ORIENTED_EDGE('',*,*,#3699,.T.);
#4918=ORIENTED_EDGE('',*,*,#3686,.T.);
#4919=ORIENTED_EDGE('',*,*,#3700,.T.);
#4920=ORIENTED_EDGE('',*,*,#3697,.F.);
#4921=ORIENTED_EDGE('',*,*,#3699,.F.);
#4922=ORIENTED_EDGE('',*,*,#3696,.F.);
#4923=ORIENTED_EDGE('',*,*,#3693,.F.);
#4924=ORIENTED_EDGE('',*,*,#3690,.F.);
#4925=ORIENTED_EDGE('',*,*,#3687,.F.);
#4926=ORIENTED_EDGE('',*,*,#3683,.F.);
#4927=ORIENTED_EDGE('',*,*,#3700,.F.);
#4928=ORIENTED_EDGE('',*,*,#3685,.F.);
#4929=ORIENTED_EDGE('',*,*,#3689,.F.);
#4930=ORIENTED_EDGE('',*,*,#3692,.F.);
#4931=ORIENTED_EDGE('',*,*,#3695,.F.);
#4932=ORIENTED_EDGE('',*,*,#3698,.F.);
#4933=ORIENTED_EDGE('',*,*,#3701,.T.);
#4934=ORIENTED_EDGE('',*,*,#3702,.F.);
#4935=ORIENTED_EDGE('',*,*,#3701,.F.);
#4936=ORIENTED_EDGE('',*,*,#3703,.T.);
#4937=ORIENTED_EDGE('',*,*,#3704,.T.);
#4938=ORIENTED_EDGE('',*,*,#3703,.F.);
#4939=ORIENTED_EDGE('',*,*,#3704,.F.);
#4940=ORIENTED_EDGE('',*,*,#3705,.F.);
#4941=ORIENTED_EDGE('',*,*,#3706,.F.);
#4942=ORIENTED_EDGE('',*,*,#3707,.T.);
#4943=ORIENTED_EDGE('',*,*,#3705,.T.);
#4944=ORIENTED_EDGE('',*,*,#3707,.F.);
#4945=ORIENTED_EDGE('',*,*,#3708,.F.);
#4946=ORIENTED_EDGE('',*,*,#3709,.T.);
#4947=ORIENTED_EDGE('',*,*,#3706,.T.);
#4948=ORIENTED_EDGE('',*,*,#3709,.F.);
#4949=ORIENTED_EDGE('',*,*,#3710,.F.);
#4950=ORIENTED_EDGE('',*,*,#3711,.T.);
#4951=ORIENTED_EDGE('',*,*,#3708,.T.);
#4952=ORIENTED_EDGE('',*,*,#3711,.F.);
#4953=ORIENTED_EDGE('',*,*,#3710,.T.);
#4954=ORIENTED_EDGE('',*,*,#3712,.F.);
#4955=ORIENTED_EDGE('',*,*,#3713,.F.);
#4956=ORIENTED_EDGE('',*,*,#3714,.T.);
#4957=ORIENTED_EDGE('',*,*,#3712,.T.);
#4958=ORIENTED_EDGE('',*,*,#3714,.F.);
#4959=ORIENTED_EDGE('',*,*,#3702,.T.);
#4960=ORIENTED_EDGE('',*,*,#3715,.T.);
#4961=ORIENTED_EDGE('',*,*,#3713,.T.);
#4962=ORIENTED_EDGE('',*,*,#3715,.F.);
#4963=ORIENTED_EDGE('',*,*,#3716,.F.);
#4964=ORIENTED_EDGE('',*,*,#3717,.F.);
#4965=ORIENTED_EDGE('',*,*,#3718,.T.);
#4966=ORIENTED_EDGE('',*,*,#3716,.T.);
#4967=ORIENTED_EDGE('',*,*,#3718,.F.);
#4968=ORIENTED_EDGE('',*,*,#3719,.F.);
#4969=ORIENTED_EDGE('',*,*,#3720,.T.);
#4970=ORIENTED_EDGE('',*,*,#3717,.T.);
#4971=ORIENTED_EDGE('',*,*,#3720,.F.);
#4972=ORIENTED_EDGE('',*,*,#3721,.F.);
#4973=ORIENTED_EDGE('',*,*,#3722,.T.);
#4974=ORIENTED_EDGE('',*,*,#3719,.T.);
#4975=ORIENTED_EDGE('',*,*,#3722,.F.);
#4976=ORIENTED_EDGE('',*,*,#3721,.T.);
#4977=ORIENTED_EDGE('',*,*,#3723,.F.);
#4978=ORIENTED_EDGE('',*,*,#3724,.F.);
#4979=ORIENTED_EDGE('',*,*,#3725,.T.);
#4980=ORIENTED_EDGE('',*,*,#3723,.T.);
#4981=ORIENTED_EDGE('',*,*,#3725,.F.);
#4982=ORIENTED_EDGE('',*,*,#3726,.F.);
#4983=ORIENTED_EDGE('',*,*,#3727,.T.);
#4984=ORIENTED_EDGE('',*,*,#3724,.T.);
#4985=ORIENTED_EDGE('',*,*,#3727,.F.);
#4986=ORIENTED_EDGE('',*,*,#3728,.F.);
#4987=ORIENTED_EDGE('',*,*,#3729,.T.);
#4988=ORIENTED_EDGE('',*,*,#3726,.T.);
#4989=ORIENTED_EDGE('',*,*,#3729,.F.);
#4990=ORIENTED_EDGE('',*,*,#3728,.T.);
#4991=ORIENTED_EDGE('',*,*,#3730,.T.);
#4992=ORIENTED_EDGE('',*,*,#3731,.T.);
#4993=ORIENTED_EDGE('',*,*,#3732,.T.);
#4994=ORIENTED_EDGE('',*,*,#3733,.F.);
#4995=ORIENTED_EDGE('',*,*,#3734,.T.);
#4996=ORIENTED_EDGE('',*,*,#3735,.T.);
#4997=ORIENTED_EDGE('',*,*,#3736,.T.);
#4998=ORIENTED_EDGE('',*,*,#3731,.F.);
#4999=ORIENTED_EDGE('',*,*,#3737,.T.);
#5000=ORIENTED_EDGE('',*,*,#3738,.T.);
#5001=ORIENTED_EDGE('',*,*,#3739,.T.);
#5002=ORIENTED_EDGE('',*,*,#3735,.F.);
#5003=ORIENTED_EDGE('',*,*,#3740,.T.);
#5004=ORIENTED_EDGE('',*,*,#3741,.T.);
#5005=ORIENTED_EDGE('',*,*,#3742,.T.);
#5006=ORIENTED_EDGE('',*,*,#3738,.F.);
#5007=ORIENTED_EDGE('',*,*,#3743,.T.);
#5008=ORIENTED_EDGE('',*,*,#3744,.T.);
#5009=ORIENTED_EDGE('',*,*,#3745,.T.);
#5010=ORIENTED_EDGE('',*,*,#3741,.F.);
#5011=ORIENTED_EDGE('',*,*,#3746,.T.);
#5012=ORIENTED_EDGE('',*,*,#3733,.T.);
#5013=ORIENTED_EDGE('',*,*,#3747,.T.);
#5014=ORIENTED_EDGE('',*,*,#3744,.F.);
#5015=ORIENTED_EDGE('',*,*,#3746,.F.);
#5016=ORIENTED_EDGE('',*,*,#3743,.F.);
#5017=ORIENTED_EDGE('',*,*,#3740,.F.);
#5018=ORIENTED_EDGE('',*,*,#3737,.F.);
#5019=ORIENTED_EDGE('',*,*,#3734,.F.);
#5020=ORIENTED_EDGE('',*,*,#3730,.F.);
#5021=ORIENTED_EDGE('',*,*,#3747,.F.);
#5022=ORIENTED_EDGE('',*,*,#3732,.F.);
#5023=ORIENTED_EDGE('',*,*,#3736,.F.);
#5024=ORIENTED_EDGE('',*,*,#3739,.F.);
#5025=ORIENTED_EDGE('',*,*,#3742,.F.);
#5026=ORIENTED_EDGE('',*,*,#3745,.F.);
#5027=ORIENTED_EDGE('',*,*,#3748,.F.);
#5028=ORIENTED_EDGE('',*,*,#3749,.F.);
#5029=ORIENTED_EDGE('',*,*,#3750,.F.);
#5030=ORIENTED_EDGE('',*,*,#3751,.F.);
#5031=ORIENTED_EDGE('',*,*,#3750,.T.);
#5032=ORIENTED_EDGE('',*,*,#3752,.T.);
#5033=ORIENTED_EDGE('',*,*,#3753,.F.);
#5034=ORIENTED_EDGE('',*,*,#3754,.F.);
#5035=ORIENTED_EDGE('',*,*,#3755,.T.);
#5036=ORIENTED_EDGE('',*,*,#3756,.T.);
#5037=ORIENTED_EDGE('',*,*,#3757,.T.);
#5038=ORIENTED_EDGE('',*,*,#3753,.T.);
#5039=ORIENTED_EDGE('',*,*,#3758,.T.);
#5040=ORIENTED_EDGE('',*,*,#3755,.F.);
#5041=ORIENTED_EDGE('',*,*,#3752,.F.);
#5042=ORIENTED_EDGE('',*,*,#3749,.T.);
#5043=ORIENTED_EDGE('',*,*,#3759,.F.);
#5044=ORIENTED_EDGE('',*,*,#3760,.F.);
#5045=ORIENTED_EDGE('',*,*,#3761,.T.);
#5046=ORIENTED_EDGE('',*,*,#3762,.F.);
#5047=ORIENTED_EDGE('',*,*,#3763,.T.);
#5048=ORIENTED_EDGE('',*,*,#3764,.T.);
#5049=ORIENTED_EDGE('',*,*,#3765,.T.);
#5050=ORIENTED_EDGE('',*,*,#3766,.T.);
#5051=ORIENTED_EDGE('',*,*,#3767,.T.);
#5052=ORIENTED_EDGE('',*,*,#3756,.F.);
#5053=ORIENTED_EDGE('',*,*,#3765,.F.);
#5054=ORIENTED_EDGE('',*,*,#3768,.F.);
#5055=ORIENTED_EDGE('',*,*,#3769,.F.);
#5056=ORIENTED_EDGE('',*,*,#3766,.F.);
#5057=ORIENTED_EDGE('',*,*,#3764,.F.);
#5058=ORIENTED_EDGE('',*,*,#3757,.F.);
#5059=ORIENTED_EDGE('',*,*,#3767,.F.);
#5060=ORIENTED_EDGE('',*,*,#3769,.T.);
#5061=ORIENTED_EDGE('',*,*,#3770,.F.);
#5062=ORIENTED_EDGE('',*,*,#3771,.F.);
#5063=ORIENTED_EDGE('',*,*,#3772,.T.);
#5064=ORIENTED_EDGE('',*,*,#3773,.F.);
#5065=ORIENTED_EDGE('',*,*,#3774,.T.);
#5066=ORIENTED_EDGE('',*,*,#3751,.T.);
#5067=ORIENTED_EDGE('',*,*,#3754,.T.);
#5068=ORIENTED_EDGE('',*,*,#3768,.T.);
#5069=ORIENTED_EDGE('',*,*,#3763,.F.);
#5070=ORIENTED_EDGE('',*,*,#3775,.F.);
#5071=ORIENTED_EDGE('',*,*,#3770,.T.);
#5072=ORIENTED_EDGE('',*,*,#3771,.T.);
#5073=ORIENTED_EDGE('',*,*,#3775,.T.);
#5074=ORIENTED_EDGE('',*,*,#3762,.T.);
#5075=ORIENTED_EDGE('',*,*,#3776,.T.);
#5076=ORIENTED_EDGE('',*,*,#3777,.T.);
#5077=ORIENTED_EDGE('',*,*,#3778,.T.);
#5078=ORIENTED_EDGE('',*,*,#3777,.F.);
#5079=ORIENTED_EDGE('',*,*,#3779,.F.);
#5080=ORIENTED_EDGE('',*,*,#3780,.T.);
#5081=ORIENTED_EDGE('',*,*,#3758,.F.);
#5082=ORIENTED_EDGE('',*,*,#3780,.F.);
#5083=ORIENTED_EDGE('',*,*,#3781,.F.);
#5084=ORIENTED_EDGE('',*,*,#3782,.F.);
#5085=ORIENTED_EDGE('',*,*,#3783,.F.);
#5086=ORIENTED_EDGE('',*,*,#3776,.F.);
#5087=ORIENTED_EDGE('',*,*,#3761,.F.);
#5088=ORIENTED_EDGE('',*,*,#3784,.F.);
#5089=ORIENTED_EDGE('',*,*,#3781,.T.);
#5090=ORIENTED_EDGE('',*,*,#3779,.T.);
#5091=ORIENTED_EDGE('',*,*,#3778,.F.);
#5092=ORIENTED_EDGE('',*,*,#3783,.T.);
#5093=ORIENTED_EDGE('',*,*,#3785,.F.);
#5094=ORIENTED_EDGE('',*,*,#3772,.F.);
#5095=ORIENTED_EDGE('',*,*,#3760,.T.);
#5096=ORIENTED_EDGE('',*,*,#3786,.T.);
#5097=ORIENTED_EDGE('',*,*,#3773,.T.);
#5098=ORIENTED_EDGE('',*,*,#3785,.T.);
#5099=ORIENTED_EDGE('',*,*,#3782,.T.);
#5100=ORIENTED_EDGE('',*,*,#3784,.T.);
#5101=ORIENTED_EDGE('',*,*,#3748,.T.);
#5102=ORIENTED_EDGE('',*,*,#3774,.F.);
#5103=ORIENTED_EDGE('',*,*,#3786,.F.);
#5104=ORIENTED_EDGE('',*,*,#3759,.T.);
#5105=ORIENTED_EDGE('',*,*,#3787,.T.);
#5106=ORIENTED_EDGE('',*,*,#3788,.T.);
#5107=ORIENTED_EDGE('',*,*,#3789,.T.);
#5108=ORIENTED_EDGE('',*,*,#3788,.F.);
#5109=ORIENTED_EDGE('',*,*,#3789,.F.);
#5110=ORIENTED_EDGE('',*,*,#3790,.T.);
#5111=ORIENTED_EDGE('',*,*,#3791,.T.);
#5112=ORIENTED_EDGE('',*,*,#3790,.F.);
#5113=ORIENTED_EDGE('',*,*,#3792,.T.);
#5114=ORIENTED_EDGE('',*,*,#3787,.F.);
#5115=ORIENTED_EDGE('',*,*,#3792,.F.);
#5116=ORIENTED_EDGE('',*,*,#3793,.T.);
#5117=ORIENTED_EDGE('',*,*,#3794,.T.);
#5118=ORIENTED_EDGE('',*,*,#3793,.F.);
#5119=ORIENTED_EDGE('',*,*,#3794,.F.);
#5120=ORIENTED_EDGE('',*,*,#3791,.F.);
#5121=ORIENTED_EDGE('',*,*,#3795,.T.);
#5122=ORIENTED_EDGE('',*,*,#3796,.T.);
#5123=ORIENTED_EDGE('',*,*,#3797,.T.);
#5124=ORIENTED_EDGE('',*,*,#3798,.F.);
#5125=ORIENTED_EDGE('',*,*,#3799,.T.);
#5126=ORIENTED_EDGE('',*,*,#3800,.T.);
#5127=ORIENTED_EDGE('',*,*,#3801,.T.);
#5128=ORIENTED_EDGE('',*,*,#3796,.F.);
#5129=ORIENTED_EDGE('',*,*,#3802,.T.);
#5130=ORIENTED_EDGE('',*,*,#3803,.T.);
#5131=ORIENTED_EDGE('',*,*,#3804,.T.);
#5132=ORIENTED_EDGE('',*,*,#3800,.F.);
#5133=ORIENTED_EDGE('',*,*,#3805,.T.);
#5134=ORIENTED_EDGE('',*,*,#3806,.T.);
#5135=ORIENTED_EDGE('',*,*,#3807,.T.);
#5136=ORIENTED_EDGE('',*,*,#3803,.F.);
#5137=ORIENTED_EDGE('',*,*,#3808,.T.);
#5138=ORIENTED_EDGE('',*,*,#3809,.T.);
#5139=ORIENTED_EDGE('',*,*,#3810,.T.);
#5140=ORIENTED_EDGE('',*,*,#3806,.F.);
#5141=ORIENTED_EDGE('',*,*,#3811,.T.);
#5142=ORIENTED_EDGE('',*,*,#3798,.T.);
#5143=ORIENTED_EDGE('',*,*,#3812,.T.);
#5144=ORIENTED_EDGE('',*,*,#3809,.F.);
#5145=ORIENTED_EDGE('',*,*,#3811,.F.);
#5146=ORIENTED_EDGE('',*,*,#3808,.F.);
#5147=ORIENTED_EDGE('',*,*,#3805,.F.);
#5148=ORIENTED_EDGE('',*,*,#3802,.F.);
#5149=ORIENTED_EDGE('',*,*,#3799,.F.);
#5150=ORIENTED_EDGE('',*,*,#3795,.F.);
#5151=ORIENTED_EDGE('',*,*,#3812,.F.);
#5152=ORIENTED_EDGE('',*,*,#3797,.F.);
#5153=ORIENTED_EDGE('',*,*,#3801,.F.);
#5154=ORIENTED_EDGE('',*,*,#3804,.F.);
#5155=ORIENTED_EDGE('',*,*,#3807,.F.);
#5156=ORIENTED_EDGE('',*,*,#3810,.F.);
#5157=ORIENTED_EDGE('',*,*,#3813,.F.);
#5158=ORIENTED_EDGE('',*,*,#3814,.F.);
#5159=ORIENTED_EDGE('',*,*,#3815,.F.);
#5160=ORIENTED_EDGE('',*,*,#3816,.T.);
#5161=ORIENTED_EDGE('',*,*,#3814,.T.);
#5162=ORIENTED_EDGE('',*,*,#3816,.F.);
#5163=ORIENTED_EDGE('',*,*,#3817,.F.);
#5164=ORIENTED_EDGE('',*,*,#3818,.T.);
#5165=ORIENTED_EDGE('',*,*,#3815,.T.);
#5166=ORIENTED_EDGE('',*,*,#3818,.F.);
#5167=ORIENTED_EDGE('',*,*,#3819,.F.);
#5168=ORIENTED_EDGE('',*,*,#3820,.T.);
#5169=ORIENTED_EDGE('',*,*,#3817,.T.);
#5170=ORIENTED_EDGE('',*,*,#3820,.F.);
#5171=ORIENTED_EDGE('',*,*,#3819,.T.);
#5172=ORIENTED_EDGE('',*,*,#3821,.F.);
#5173=ORIENTED_EDGE('',*,*,#3822,.F.);
#5174=ORIENTED_EDGE('',*,*,#3823,.T.);
#5175=ORIENTED_EDGE('',*,*,#3821,.T.);
#5176=ORIENTED_EDGE('',*,*,#3823,.F.);
#5177=ORIENTED_EDGE('',*,*,#3813,.T.);
#5178=ORIENTED_EDGE('',*,*,#3824,.T.);
#5179=ORIENTED_EDGE('',*,*,#3822,.T.);
#5180=ORIENTED_EDGE('',*,*,#3824,.F.);
#5181=ORIENTED_EDGE('',*,*,#3825,.T.);
#5182=ORIENTED_EDGE('',*,*,#3826,.T.);
#5183=ORIENTED_EDGE('',*,*,#3827,.T.);
#5184=ORIENTED_EDGE('',*,*,#3826,.F.);
#5185=ORIENTED_EDGE('',*,*,#3827,.F.);
#5186=ORIENTED_EDGE('',*,*,#3828,.T.);
#5187=ORIENTED_EDGE('',*,*,#3829,.T.);
#5188=ORIENTED_EDGE('',*,*,#3828,.F.);
#5189=ORIENTED_EDGE('',*,*,#3830,.T.);
#5190=ORIENTED_EDGE('',*,*,#3825,.F.);
#5191=ORIENTED_EDGE('',*,*,#3830,.F.);
#5192=ORIENTED_EDGE('',*,*,#3831,.T.);
#5193=ORIENTED_EDGE('',*,*,#3832,.T.);
#5194=ORIENTED_EDGE('',*,*,#3831,.F.);
#5195=ORIENTED_EDGE('',*,*,#3832,.F.);
#5196=ORIENTED_EDGE('',*,*,#3829,.F.);
#5197=ORIENTED_EDGE('',*,*,#3833,.F.);
#5198=ORIENTED_EDGE('',*,*,#3834,.F.);
#5199=ORIENTED_EDGE('',*,*,#3835,.T.);
#5200=ORIENTED_EDGE('',*,*,#3833,.T.);
#5201=ORIENTED_EDGE('',*,*,#3835,.F.);
#5202=ORIENTED_EDGE('',*,*,#3836,.F.);
#5203=ORIENTED_EDGE('',*,*,#3837,.T.);
#5204=ORIENTED_EDGE('',*,*,#3834,.T.);
#5205=ORIENTED_EDGE('',*,*,#3837,.F.);
#5206=ORIENTED_EDGE('',*,*,#3838,.F.);
#5207=ORIENTED_EDGE('',*,*,#3839,.T.);
#5208=ORIENTED_EDGE('',*,*,#3836,.T.);
#5209=ORIENTED_EDGE('',*,*,#3839,.F.);
#5210=ORIENTED_EDGE('',*,*,#3838,.T.);
#5211=ORIENTED_EDGE('',*,*,#3840,.F.);
#5212=ORIENTED_EDGE('',*,*,#3841,.F.);
#5213=ORIENTED_EDGE('',*,*,#3842,.T.);
#5214=ORIENTED_EDGE('',*,*,#3840,.T.);
#5215=ORIENTED_EDGE('',*,*,#3842,.F.);
#5216=ORIENTED_EDGE('',*,*,#3843,.F.);
#5217=ORIENTED_EDGE('',*,*,#3844,.T.);
#5218=ORIENTED_EDGE('',*,*,#3841,.T.);
#5219=ORIENTED_EDGE('',*,*,#3844,.F.);
#5220=ORIENTED_EDGE('',*,*,#3845,.F.);
#5221=ORIENTED_EDGE('',*,*,#3846,.T.);
#5222=ORIENTED_EDGE('',*,*,#3843,.T.);
#5223=ORIENTED_EDGE('',*,*,#3846,.F.);
#5224=ORIENTED_EDGE('',*,*,#3845,.T.);
#5225=ORIENTED_EDGE('',*,*,#3847,.T.);
#5226=ORIENTED_EDGE('',*,*,#3848,.T.);
#5227=ORIENTED_EDGE('',*,*,#3849,.T.);
#5228=ORIENTED_EDGE('',*,*,#3850,.F.);
#5229=ORIENTED_EDGE('',*,*,#3851,.T.);
#5230=ORIENTED_EDGE('',*,*,#3852,.T.);
#5231=ORIENTED_EDGE('',*,*,#3853,.T.);
#5232=ORIENTED_EDGE('',*,*,#3848,.F.);
#5233=ORIENTED_EDGE('',*,*,#3854,.T.);
#5234=ORIENTED_EDGE('',*,*,#3855,.T.);
#5235=ORIENTED_EDGE('',*,*,#3856,.T.);
#5236=ORIENTED_EDGE('',*,*,#3852,.F.);
#5237=ORIENTED_EDGE('',*,*,#3857,.T.);
#5238=ORIENTED_EDGE('',*,*,#3858,.T.);
#5239=ORIENTED_EDGE('',*,*,#3859,.T.);
#5240=ORIENTED_EDGE('',*,*,#3855,.F.);
#5241=ORIENTED_EDGE('',*,*,#3860,.T.);
#5242=ORIENTED_EDGE('',*,*,#3861,.T.);
#5243=ORIENTED_EDGE('',*,*,#3862,.T.);
#5244=ORIENTED_EDGE('',*,*,#3858,.F.);
#5245=ORIENTED_EDGE('',*,*,#3863,.T.);
#5246=ORIENTED_EDGE('',*,*,#3850,.T.);
#5247=ORIENTED_EDGE('',*,*,#3864,.T.);
#5248=ORIENTED_EDGE('',*,*,#3861,.F.);
#5249=ORIENTED_EDGE('',*,*,#3863,.F.);
#5250=ORIENTED_EDGE('',*,*,#3860,.F.);
#5251=ORIENTED_EDGE('',*,*,#3857,.F.);
#5252=ORIENTED_EDGE('',*,*,#3854,.F.);
#5253=ORIENTED_EDGE('',*,*,#3851,.F.);
#5254=ORIENTED_EDGE('',*,*,#3847,.F.);
#5255=ORIENTED_EDGE('',*,*,#3864,.F.);
#5256=ORIENTED_EDGE('',*,*,#3849,.F.);
#5257=ORIENTED_EDGE('',*,*,#3853,.F.);
#5258=ORIENTED_EDGE('',*,*,#3856,.F.);
#5259=ORIENTED_EDGE('',*,*,#3859,.F.);
#5260=ORIENTED_EDGE('',*,*,#3862,.F.);
#5261=CYLINDRICAL_SURFACE('',#5884,0.274999999999999);
#5262=CYLINDRICAL_SURFACE('',#5887,2.);
#5263=CYLINDRICAL_SURFACE('',#5893,0.600000000000001);
#5264=CYLINDRICAL_SURFACE('',#5896,2.);
#5265=CYLINDRICAL_SURFACE('',#5902,0.274999999999999);
#5266=CYLINDRICAL_SURFACE('',#5905,2.);
#5267=CYLINDRICAL_SURFACE('',#5911,0.600000000000001);
#5268=CYLINDRICAL_SURFACE('',#5914,2.);
#5269=CYLINDRICAL_SURFACE('',#5920,0.274999999999999);
#5270=CYLINDRICAL_SURFACE('',#5923,2.);
#5271=CYLINDRICAL_SURFACE('',#5929,0.600000000000001);
#5272=CYLINDRICAL_SURFACE('',#5932,2.);
#5273=CYLINDRICAL_SURFACE('',#5938,0.274999999999999);
#5274=CYLINDRICAL_SURFACE('',#5941,2.);
#5275=CYLINDRICAL_SURFACE('',#5947,0.600000000000001);
#5276=CYLINDRICAL_SURFACE('',#5950,2.);
#5277=CYLINDRICAL_SURFACE('',#5956,0.5);
#5278=CYLINDRICAL_SURFACE('',#5961,0.5);
#5279=CYLINDRICAL_SURFACE('',#5966,0.5);
#5280=CYLINDRICAL_SURFACE('',#5971,0.5);
#5281=CYLINDRICAL_SURFACE('',#5976,0.274999999999999);
#5282=CYLINDRICAL_SURFACE('',#5978,0.274999999999999);
#5283=CYLINDRICAL_SURFACE('',#5980,0.274999999999999);
#5284=CYLINDRICAL_SURFACE('',#5982,0.274999999999999);
#5285=CYLINDRICAL_SURFACE('',#5991,0.274999999999999);
#5286=CYLINDRICAL_SURFACE('',#5994,0.274999999999999);
#5287=CYLINDRICAL_SURFACE('',#5997,0.274999999999999);
#5288=CYLINDRICAL_SURFACE('',#6000,0.274999999999999);
#5289=CYLINDRICAL_SURFACE('',#6018,0.164999999999999);
#5290=CYLINDRICAL_SURFACE('',#6021,0.275);
#5291=CYLINDRICAL_SURFACE('',#6024,0.275);
#5292=CYLINDRICAL_SURFACE('',#6036,0.164999999999999);
#5293=CYLINDRICAL_SURFACE('',#6039,0.275);
#5294=CYLINDRICAL_SURFACE('',#6042,0.275);
#5295=CYLINDRICAL_SURFACE('',#6054,0.225);
#5296=CYLINDRICAL_SURFACE('',#6057,0.225);
#5297=CYLINDRICAL_SURFACE('',#6067,0.275);
#5298=CYLINDRICAL_SURFACE('',#6070,0.274999999999999);
#5299=CYLINDRICAL_SURFACE('',#6073,0.21);
#5300=CYLINDRICAL_SURFACE('',#6074,0.21);
#5301=CYLINDRICAL_SURFACE('',#6075,0.275);
#5302=CYLINDRICAL_SURFACE('',#6078,0.274999999999999);
#5303=CYLINDRICAL_SURFACE('',#6081,0.21);
#5304=CYLINDRICAL_SURFACE('',#6082,0.21);
#5305=CYLINDRICAL_SURFACE('',#6120,0.21);
#5306=CYLINDRICAL_SURFACE('',#6175,0.21);
#5307=CYLINDRICAL_SURFACE('',#6194,0.25);
#5308=CYLINDRICAL_SURFACE('',#6201,0.425);
#5309=CYLINDRICAL_SURFACE('',#6209,0.24505);
#5310=CYLINDRICAL_SURFACE('',#6215,0.425);
#5311=CYLINDRICAL_SURFACE('',#6223,0.24505);
#5312=CYLINDRICAL_SURFACE('',#6248,0.2117);
#5313=CYLINDRICAL_SURFACE('',#6261,0.265);
#5314=CYLINDRICAL_SURFACE('',#6265,0.5);
#5315=CYLINDRICAL_SURFACE('',#6283,0.425);
#5316=CYLINDRICAL_SURFACE('',#6291,0.24505);
#5317=CYLINDRICAL_SURFACE('',#6296,0.215);
#5318=CYLINDRICAL_SURFACE('',#6300,0.45);
#5319=CYLINDRICAL_SURFACE('',#6308,0.35);
#5320=CYLINDRICAL_SURFACE('',#6316,0.1954);
#5321=ADVANCED_FACE('',(#825),#5261,.F.);
#5322=ADVANCED_FACE('',(#826),#5262,.T.);
#5323=ADVANCED_FACE('',(#827,#531),#609,.T.);
#5324=ADVANCED_FACE('',(#828,#532),#610,.F.);
#5325=ADVANCED_FACE('',(#829),#5263,.F.);
#5326=ADVANCED_FACE('',(#830),#5264,.T.);
#5327=ADVANCED_FACE('',(#831,#533),#611,.T.);
#5328=ADVANCED_FACE('',(#832,#534),#612,.F.);
#5329=ADVANCED_FACE('',(#833),#5265,.F.);
#5330=ADVANCED_FACE('',(#834),#5266,.T.);
#5331=ADVANCED_FACE('',(#835,#535),#613,.T.);
#5332=ADVANCED_FACE('',(#836,#536),#614,.F.);
#5333=ADVANCED_FACE('',(#837),#5267,.F.);
#5334=ADVANCED_FACE('',(#838),#5268,.T.);
#5335=ADVANCED_FACE('',(#839,#537),#615,.T.);
#5336=ADVANCED_FACE('',(#840,#538),#616,.F.);
#5337=ADVANCED_FACE('',(#841),#5269,.F.);
#5338=ADVANCED_FACE('',(#842),#5270,.T.);
#5339=ADVANCED_FACE('',(#843,#539),#617,.T.);
#5340=ADVANCED_FACE('',(#844,#540),#618,.F.);
#5341=ADVANCED_FACE('',(#845),#5271,.F.);
#5342=ADVANCED_FACE('',(#846),#5272,.T.);
#5343=ADVANCED_FACE('',(#847,#541),#619,.T.);
#5344=ADVANCED_FACE('',(#848,#542),#620,.F.);
#5345=ADVANCED_FACE('',(#849),#5273,.F.);
#5346=ADVANCED_FACE('',(#850),#5274,.T.);
#5347=ADVANCED_FACE('',(#851,#543),#621,.T.);
#5348=ADVANCED_FACE('',(#852,#544),#622,.F.);
#5349=ADVANCED_FACE('',(#853),#5275,.F.);
#5350=ADVANCED_FACE('',(#854),#5276,.T.);
#5351=ADVANCED_FACE('',(#855,#545),#623,.T.);
#5352=ADVANCED_FACE('',(#856,#546),#624,.F.);
#5353=ADVANCED_FACE('',(#857),#5277,.F.);
#5354=ADVANCED_FACE('',(#858,#547),#625,.T.);
#5355=ADVANCED_FACE('',(#859),#5278,.F.);
#5356=ADVANCED_FACE('',(#860,#548),#626,.T.);
#5357=ADVANCED_FACE('',(#861),#5279,.F.);
#5358=ADVANCED_FACE('',(#862,#549),#627,.T.);
#5359=ADVANCED_FACE('',(#863),#5280,.F.);
#5360=ADVANCED_FACE('',(#864,#550),#628,.T.);
#5361=ADVANCED_FACE('',(#865),#5281,.F.);
#5362=ADVANCED_FACE('',(#866),#5282,.F.);
#5363=ADVANCED_FACE('',(#867),#5283,.F.);
#5364=ADVANCED_FACE('',(#868),#5284,.F.);
#5365=ADVANCED_FACE('',(#869),#629,.T.);
#5366=ADVANCED_FACE('',(#870),#630,.T.);
#5367=ADVANCED_FACE('',(#871),#631,.T.);
#5368=ADVANCED_FACE('',(#872),#632,.T.);
#5369=ADVANCED_FACE('',(#873,#551,#552,#553,#554),#633,.T.);
#5370=ADVANCED_FACE('',(#874,#555,#556,#557,#558),#634,.F.);
#5371=ADVANCED_FACE('',(#875),#5285,.F.);
#5372=ADVANCED_FACE('',(#876),#5286,.F.);
#5373=ADVANCED_FACE('',(#877),#5287,.F.);
#5374=ADVANCED_FACE('',(#878),#5288,.F.);
#5375=ADVANCED_FACE('',(#879),#635,.F.);
#5376=ADVANCED_FACE('',(#880),#636,.F.);
#5377=ADVANCED_FACE('',(#881),#637,.T.);
#5378=ADVANCED_FACE('',(#882,#559,#560,#561,#562),#638,.T.);
#5379=ADVANCED_FACE('',(#883),#639,.F.);
#5380=ADVANCED_FACE('',(#884),#640,.F.);
#5381=ADVANCED_FACE('',(#885),#641,.T.);
#5382=ADVANCED_FACE('',(#886),#642,.F.);
#5383=ADVANCED_FACE('',(#887),#643,.F.);
#5384=ADVANCED_FACE('',(#888),#644,.T.);
#5385=ADVANCED_FACE('',(#889),#645,.F.);
#5386=ADVANCED_FACE('',(#890),#646,.F.);
#5387=ADVANCED_FACE('',(#891),#647,.T.);
#5388=ADVANCED_FACE('',(#892,#563,#564,#565,#566),#648,.F.);
#5389=ADVANCED_FACE('',(#893),#5289,.F.);
#5390=ADVANCED_FACE('',(#894),#5290,.F.);
#5391=ADVANCED_FACE('',(#895),#5291,.F.);
#5392=ADVANCED_FACE('',(#896,#567),#649,.T.);
#5393=ADVANCED_FACE('',(#897),#650,.T.);
#5394=ADVANCED_FACE('',(#898,#568),#651,.T.);
#5395=ADVANCED_FACE('',(#899,#569,#570),#652,.T.);
#5396=ADVANCED_FACE('',(#900),#653,.T.);
#5397=ADVANCED_FACE('',(#901,#571,#572),#654,.T.);
#5398=ADVANCED_FACE('',(#902),#655,.T.);
#5399=ADVANCED_FACE('',(#903),#656,.F.);
#5400=ADVANCED_FACE('',(#904),#5292,.F.);
#5401=ADVANCED_FACE('',(#905),#5293,.F.);
#5402=ADVANCED_FACE('',(#906),#5294,.F.);
#5403=ADVANCED_FACE('',(#907,#573),#657,.T.);
#5404=ADVANCED_FACE('',(#908),#658,.T.);
#5405=ADVANCED_FACE('',(#909,#574),#659,.T.);
#5406=ADVANCED_FACE('',(#910,#575,#576),#660,.T.);
#5407=ADVANCED_FACE('',(#911),#661,.T.);
#5408=ADVANCED_FACE('',(#912,#577,#578),#662,.T.);
#5409=ADVANCED_FACE('',(#913),#663,.T.);
#5410=ADVANCED_FACE('',(#914),#664,.F.);
#5411=ADVANCED_FACE('',(#915),#5295,.F.);
#5412=ADVANCED_FACE('',(#916),#5296,.F.);
#5413=ADVANCED_FACE('',(#917),#665,.T.);
#5414=ADVANCED_FACE('',(#918),#666,.T.);
#5415=ADVANCED_FACE('',(#919),#667,.T.);
#5416=ADVANCED_FACE('',(#920),#668,.T.);
#5417=ADVANCED_FACE('',(#921,#579,#580),#669,.T.);
#5418=ADVANCED_FACE('',(#922,#581,#582),#670,.F.);
#5419=ADVANCED_FACE('',(#923,#583),#5297,.F.);
#5420=ADVANCED_FACE('',(#924,#584),#5298,.F.);
#5421=ADVANCED_FACE('',(#925),#5299,.F.);
#5422=ADVANCED_FACE('',(#926),#5300,.F.);
#5423=ADVANCED_FACE('',(#927,#585),#5301,.F.);
#5424=ADVANCED_FACE('',(#928,#586),#5302,.F.);
#5425=ADVANCED_FACE('',(#929),#5303,.F.);
#5426=ADVANCED_FACE('',(#930),#5304,.F.);
#5427=ADVANCED_FACE('',(#931),#671,.F.);
#5428=ADVANCED_FACE('',(#932),#672,.F.);
#5429=ADVANCED_FACE('',(#933),#673,.F.);
#5430=ADVANCED_FACE('',(#934),#674,.F.);
#5431=ADVANCED_FACE('',(#935,#587,#588),#675,.F.);
#5432=ADVANCED_FACE('',(#936),#676,.F.);
#5433=ADVANCED_FACE('',(#937),#677,.F.);
#5434=ADVANCED_FACE('',(#938),#678,.F.);
#5435=ADVANCED_FACE('',(#939),#679,.F.);
#5436=ADVANCED_FACE('',(#940),#680,.F.);
#5437=ADVANCED_FACE('',(#941),#681,.F.);
#5438=ADVANCED_FACE('',(#942),#682,.F.);
#5439=ADVANCED_FACE('',(#943),#683,.F.);
#5440=ADVANCED_FACE('',(#944,#589,#590),#684,.F.);
#5441=ADVANCED_FACE('',(#945),#685,.F.);
#5442=ADVANCED_FACE('',(#946),#686,.F.);
#5443=ADVANCED_FACE('',(#947),#687,.F.);
#5444=ADVANCED_FACE('',(#948),#688,.F.);
#5445=ADVANCED_FACE('',(#949),#689,.F.);
#5446=ADVANCED_FACE('',(#950),#690,.F.);
#5447=ADVANCED_FACE('',(#951),#691,.F.);
#5448=ADVANCED_FACE('',(#952),#692,.F.);
#5449=ADVANCED_FACE('',(#953,#591,#592),#693,.F.);
#5450=ADVANCED_FACE('',(#954),#694,.F.);
#5451=ADVANCED_FACE('',(#955),#695,.F.);
#5452=ADVANCED_FACE('',(#956),#696,.F.);
#5453=ADVANCED_FACE('',(#957),#697,.F.);
#5454=ADVANCED_FACE('',(#958),#698,.F.);
#5455=ADVANCED_FACE('',(#959),#699,.F.);
#5456=ADVANCED_FACE('',(#960),#700,.F.);
#5457=ADVANCED_FACE('',(#961),#701,.F.);
#5458=ADVANCED_FACE('',(#962,#593,#594),#702,.F.);
#5459=ADVANCED_FACE('',(#963),#703,.F.);
#5460=ADVANCED_FACE('',(#964),#704,.F.);
#5461=ADVANCED_FACE('',(#965),#705,.F.);
#5462=ADVANCED_FACE('',(#966),#706,.F.);
#5463=ADVANCED_FACE('',(#967),#5305,.F.);
#5464=ADVANCED_FACE('',(#968),#707,.T.);
#5465=ADVANCED_FACE('',(#969),#708,.T.);
#5466=ADVANCED_FACE('',(#970),#709,.T.);
#5467=ADVANCED_FACE('',(#971),#710,.T.);
#5468=ADVANCED_FACE('',(#972),#711,.T.);
#5469=ADVANCED_FACE('',(#973),#712,.T.);
#5470=ADVANCED_FACE('',(#974),#713,.T.);
#5471=ADVANCED_FACE('',(#975),#714,.T.);
#5472=ADVANCED_FACE('',(#976,#595),#715,.T.);
#5473=ADVANCED_FACE('',(#977,#596),#716,.F.);
#5474=ADVANCED_FACE('',(#978,#597),#717,.T.);
#5475=ADVANCED_FACE('',(#979),#718,.F.);
#5476=ADVANCED_FACE('',(#980),#719,.T.);
#5477=ADVANCED_FACE('',(#981),#720,.T.);
#5478=ADVANCED_FACE('',(#982),#721,.F.);
#5479=ADVANCED_FACE('',(#983),#722,.F.);
#5480=ADVANCED_FACE('',(#984),#723,.F.);
#5481=ADVANCED_FACE('',(#985),#724,.F.);
#5482=ADVANCED_FACE('',(#986),#725,.F.);
#5483=ADVANCED_FACE('',(#987),#726,.F.);
#5484=ADVANCED_FACE('',(#988),#727,.F.);
#5485=ADVANCED_FACE('',(#989),#728,.F.);
#5486=ADVANCED_FACE('',(#990),#729,.F.);
#5487=ADVANCED_FACE('',(#991),#730,.T.);
#5488=ADVANCED_FACE('',(#992),#731,.T.);
#5489=ADVANCED_FACE('',(#993),#732,.F.);
#5490=ADVANCED_FACE('',(#994),#733,.F.);
#5491=ADVANCED_FACE('',(#995),#734,.F.);
#5492=ADVANCED_FACE('',(#996),#735,.F.);
#5493=ADVANCED_FACE('',(#997),#736,.F.);
#5494=ADVANCED_FACE('',(#998),#737,.F.);
#5495=ADVANCED_FACE('',(#999),#738,.F.);
#5496=ADVANCED_FACE('',(#1000),#739,.F.);
#5497=ADVANCED_FACE('',(#1001),#740,.F.);
#5498=ADVANCED_FACE('',(#1002),#741,.F.);
#5499=ADVANCED_FACE('',(#1003),#742,.F.);
#5500=ADVANCED_FACE('',(#1004),#743,.F.);
#5501=ADVANCED_FACE('',(#1005),#744,.F.);
#5502=ADVANCED_FACE('',(#1006),#745,.F.);
#5503=ADVANCED_FACE('',(#1007),#746,.F.);
#5504=ADVANCED_FACE('',(#1008),#747,.F.);
#5505=ADVANCED_FACE('',(#1009),#748,.F.);
#5506=ADVANCED_FACE('',(#1010),#749,.F.);
#5507=ADVANCED_FACE('',(#1011),#750,.F.);
#5508=ADVANCED_FACE('',(#1012),#751,.F.);
#5509=ADVANCED_FACE('',(#1013),#752,.F.);
#5510=ADVANCED_FACE('',(#1014),#753,.F.);
#5511=ADVANCED_FACE('',(#1015),#754,.F.);
#5512=ADVANCED_FACE('',(#1016),#755,.F.);
#5513=ADVANCED_FACE('',(#1017),#756,.F.);
#5514=ADVANCED_FACE('',(#1018),#757,.F.);
#5515=ADVANCED_FACE('',(#1019),#5306,.F.);
#5516=ADVANCED_FACE('',(#1020),#758,.T.);
#5517=ADVANCED_FACE('',(#1021),#759,.T.);
#5518=ADVANCED_FACE('',(#1022),#760,.T.);
#5519=ADVANCED_FACE('',(#1023),#761,.T.);
#5520=ADVANCED_FACE('',(#1024,#598),#762,.F.);
#5521=ADVANCED_FACE('',(#1025),#763,.F.);
#5522=ADVANCED_FACE('',(#1026),#764,.F.);
#5523=ADVANCED_FACE('',(#1027),#765,.F.);
#5524=ADVANCED_FACE('',(#1028),#766,.F.);
#5525=ADVANCED_FACE('',(#1029),#767,.F.);
#5526=ADVANCED_FACE('',(#1030),#768,.F.);
#5527=ADVANCED_FACE('',(#1031),#769,.F.);
#5528=ADVANCED_FACE('',(#1032),#770,.F.);
#5529=ADVANCED_FACE('',(#1033,#599),#771,.T.);
#5530=ADVANCED_FACE('',(#1034),#5307,.T.);
#5531=ADVANCED_FACE('',(#1035),#772,.F.);
#5532=ADVANCED_FACE('',(#1036),#773,.T.);
#5533=ADVANCED_FACE('',(#1037),#401,.T.);
#5534=ADVANCED_FACE('',(#1038),#5308,.T.);
#5535=ADVANCED_FACE('',(#1039),#402,.T.);
#5536=ADVANCED_FACE('',(#1040,#600),#774,.T.);
#5537=ADVANCED_FACE('',(#1041),#403,.T.);
#5538=ADVANCED_FACE('',(#1042),#5309,.T.);
#5539=ADVANCED_FACE('',(#1043),#775,.T.);
#5540=ADVANCED_FACE('',(#1044),#404,.T.);
#5541=ADVANCED_FACE('',(#1045),#5310,.T.);
#5542=ADVANCED_FACE('',(#1046),#405,.T.);
#5543=ADVANCED_FACE('',(#1047,#601),#776,.T.);
#5544=ADVANCED_FACE('',(#1048),#406,.T.);
#5545=ADVANCED_FACE('',(#1049),#5311,.T.);
#5546=ADVANCED_FACE('',(#1050),#407,.T.);
#5547=ADVANCED_FACE('',(#1051),#777,.T.);
#5548=ADVANCED_FACE('',(#1052),#778,.F.);
#5549=ADVANCED_FACE('',(#1053),#779,.F.);
#5550=ADVANCED_FACE('',(#1054),#780,.F.);
#5551=ADVANCED_FACE('',(#1055),#781,.F.);
#5552=ADVANCED_FACE('',(#1056),#782,.F.);
#5553=ADVANCED_FACE('',(#1057),#783,.F.);
#5554=ADVANCED_FACE('',(#1058),#784,.F.);
#5555=ADVANCED_FACE('',(#1059),#785,.F.);
#5556=ADVANCED_FACE('',(#1060),#786,.F.);
#5557=ADVANCED_FACE('',(#1061),#787,.T.);
#5558=ADVANCED_FACE('',(#1062,#602),#788,.T.);
#5559=ADVANCED_FACE('',(#1063),#789,.T.);
#5560=ADVANCED_FACE('',(#1064),#790,.T.);
#5561=ADVANCED_FACE('',(#1065),#791,.F.);
#5562=ADVANCED_FACE('',(#1066),#792,.T.);
#5563=ADVANCED_FACE('',(#1067),#793,.T.);
#5564=ADVANCED_FACE('',(#1068),#794,.T.);
#5565=ADVANCED_FACE('',(#1069),#5312,.F.);
#5566=ADVANCED_FACE('',(#1070),#795,.F.);
#5567=ADVANCED_FACE('',(#1071),#796,.F.);
#5568=ADVANCED_FACE('',(#1072),#797,.T.);
#5569=ADVANCED_FACE('',(#1073),#798,.T.);
#5570=ADVANCED_FACE('',(#1074),#408,.F.);
#5571=ADVANCED_FACE('',(#1075),#5313,.F.);
#5572=ADVANCED_FACE('',(#1076,#603),#799,.T.);
#5573=ADVANCED_FACE('',(#1077),#5314,.T.);
#5574=ADVANCED_FACE('',(#1078,#604),#800,.F.);
#5575=ADVANCED_FACE('',(#1079),#801,.F.);
#5576=ADVANCED_FACE('',(#1080),#802,.F.);
#5577=ADVANCED_FACE('',(#1081),#803,.F.);
#5578=ADVANCED_FACE('',(#1082),#804,.F.);
#5579=ADVANCED_FACE('',(#1083),#805,.F.);
#5580=ADVANCED_FACE('',(#1084),#806,.F.);
#5581=ADVANCED_FACE('',(#1085),#807,.F.);
#5582=ADVANCED_FACE('',(#1086),#808,.F.);
#5583=ADVANCED_FACE('',(#1087),#809,.F.);
#5584=ADVANCED_FACE('',(#1088),#810,.T.);
#5585=ADVANCED_FACE('',(#1089),#409,.T.);
#5586=ADVANCED_FACE('',(#1090),#5315,.T.);
#5587=ADVANCED_FACE('',(#1091),#410,.T.);
#5588=ADVANCED_FACE('',(#1092,#605),#811,.T.);
#5589=ADVANCED_FACE('',(#1093),#411,.T.);
#5590=ADVANCED_FACE('',(#1094),#5316,.T.);
#5591=ADVANCED_FACE('',(#1095),#412,.F.);
#5592=ADVANCED_FACE('',(#1096),#5317,.F.);
#5593=ADVANCED_FACE('',(#1097,#606),#812,.T.);
#5594=ADVANCED_FACE('',(#1098),#5318,.T.);
#5595=ADVANCED_FACE('',(#1099,#607),#813,.F.);
#5596=ADVANCED_FACE('',(#1100),#814,.T.);
#5597=ADVANCED_FACE('',(#1101),#413,.T.);
#5598=ADVANCED_FACE('',(#1102),#5319,.T.);
#5599=ADVANCED_FACE('',(#1103),#414,.T.);
#5600=ADVANCED_FACE('',(#1104,#608),#815,.T.);
#5601=ADVANCED_FACE('',(#1105),#415,.T.);
#5602=ADVANCED_FACE('',(#1106),#5320,.T.);
#5603=ADVANCED_FACE('',(#1107),#416,.T.);
#5604=ADVANCED_FACE('',(#1108),#816,.T.);
#5605=ADVANCED_FACE('',(#1109),#817,.F.);
#5606=ADVANCED_FACE('',(#1110),#818,.F.);
#5607=ADVANCED_FACE('',(#1111),#819,.F.);
#5608=ADVANCED_FACE('',(#1112),#820,.F.);
#5609=ADVANCED_FACE('',(#1113),#821,.F.);
#5610=ADVANCED_FACE('',(#1114),#822,.F.);
#5611=ADVANCED_FACE('',(#1115),#823,.F.);
#5612=ADVANCED_FACE('',(#1116),#824,.F.);
#5613=CLOSED_SHELL('',(#5321,#5322,#5323,#5324));
#5614=CLOSED_SHELL('',(#5325,#5326,#5327,#5328));
#5615=CLOSED_SHELL('',(#5329,#5330,#5331,#5332));
#5616=CLOSED_SHELL('',(#5333,#5334,#5335,#5336));
#5617=CLOSED_SHELL('',(#5337,#5338,#5339,#5340));
#5618=CLOSED_SHELL('',(#5341,#5342,#5343,#5344));
#5619=CLOSED_SHELL('',(#5345,#5346,#5347,#5348));
#5620=CLOSED_SHELL('',(#5349,#5350,#5351,#5352));
#5621=CLOSED_SHELL('',(#5353,#5354,#5355,#5356,#5357,#5358,#5359,#5360,
#5361,#5362,#5363,#5364,#5365,#5366,#5367,#5368,#5369,#5370));
#5622=CLOSED_SHELL('',(#5371,#5372,#5373,#5374,#5375,#5376,#5377,#5378,
#5379,#5380,#5381,#5382,#5383,#5384,#5385,#5386,#5387,#5388));
#5623=CLOSED_SHELL('',(#5389,#5390,#5391,#5392,#5393,#5394,#5395,#5396,
#5397,#5398,#5399));
#5624=CLOSED_SHELL('',(#5400,#5401,#5402,#5403,#5404,#5405,#5406,#5407,
#5408,#5409,#5410));
#5625=CLOSED_SHELL('',(#5411,#5412,#5413,#5414,#5415,#5416,#5417,#5418));
#5626=CLOSED_SHELL('',(#5419,#5420,#5421,#5422,#5423,#5424,#5425,#5426,
#5427,#5428,#5429,#5430,#5431,#5432,#5433,#5434,#5435,#5436,#5437,#5438,
#5439,#5440,#5441,#5442,#5443,#5444,#5445,#5446,#5447,#5448,#5449,#5450,
#5451,#5452,#5453,#5454,#5455,#5456,#5457,#5458,#5459,#5460,#5461,#5462,
#5463,#5464,#5465,#5466,#5467,#5468,#5469,#5470,#5471,#5472,#5473));
#5627=CLOSED_SHELL('',(#5474,#5475,#5476,#5477,#5478,#5479,#5480,#5481,
#5482,#5483,#5484,#5485,#5486,#5487,#5488,#5489,#5490,#5491,#5492,#5493,
#5494,#5495,#5496,#5497,#5498,#5499,#5500,#5501,#5502,#5503,#5504,#5505,
#5506,#5507,#5508,#5509,#5510,#5511,#5512,#5513,#5514,#5515,#5516,#5517,
#5518,#5519,#5520));
#5628=CLOSED_SHELL('',(#5521,#5522,#5523,#5524,#5525,#5526,#5527,#5528));
#5629=CLOSED_SHELL('',(#5529,#5530,#5531,#5532,#5533,#5534,#5535,#5536,
#5537,#5538));
#5630=CLOSED_SHELL('',(#5539,#5540,#5541,#5542,#5543,#5544,#5545,#5546,
#5547));
#5631=CLOSED_SHELL('',(#5548,#5549,#5550,#5551,#5552,#5553,#5554,#5555));
#5632=CLOSED_SHELL('',(#5556,#5557,#5558,#5559,#5560,#5561,#5562,#5563,
#5564,#5565,#5566,#5567,#5568,#5569));
#5633=CLOSED_SHELL('',(#5570,#5571,#5572,#5573,#5574));
#5634=CLOSED_SHELL('',(#5575,#5576,#5577,#5578,#5579,#5580,#5581,#5582));
#5635=CLOSED_SHELL('',(#5583,#5584,#5585,#5586,#5587,#5588,#5589,#5590));
#5636=CLOSED_SHELL('',(#5591,#5592,#5593,#5594,#5595));
#5637=CLOSED_SHELL('',(#5596,#5597,#5598,#5599,#5600,#5601,#5602,#5603,
#5604));
#5638=CLOSED_SHELL('',(#5605,#5606,#5607,#5608,#5609,#5610,#5611,#5612));
#5639=DERIVED_UNIT_ELEMENT(#5683,1.);
#5640=DERIVED_UNIT_ELEMENT(#10021,-3.);
#5641=DERIVED_UNIT_ELEMENT(#5683,1.);
#5642=DERIVED_UNIT_ELEMENT(#10021,-3.);
#5643=DERIVED_UNIT_ELEMENT(#5683,1.);
#5644=DERIVED_UNIT_ELEMENT(#10021,-3.);
#5645=DERIVED_UNIT_ELEMENT(#5683,1.);
#5646=DERIVED_UNIT_ELEMENT(#10021,-3.);
#5647=DERIVED_UNIT_ELEMENT(#5683,1.);
#5648=DERIVED_UNIT_ELEMENT(#10021,-3.);
#5649=DERIVED_UNIT_ELEMENT(#5683,1.);
#5650=DERIVED_UNIT_ELEMENT(#10021,-3.);
#5651=DERIVED_UNIT_ELEMENT(#5683,1.);
#5652=DERIVED_UNIT_ELEMENT(#10021,-3.);
#5653=DERIVED_UNIT_ELEMENT(#5683,1.);
#5654=DERIVED_UNIT_ELEMENT(#10021,-3.);
#5655=DERIVED_UNIT_ELEMENT(#5683,1.);
#5656=DERIVED_UNIT_ELEMENT(#10021,-3.);
#5657=DERIVED_UNIT_ELEMENT(#5683,1.);
#5658=DERIVED_UNIT_ELEMENT(#10021,-3.);
#5659=DERIVED_UNIT_ELEMENT(#5683,1.);
#5660=DERIVED_UNIT_ELEMENT(#10021,-3.);
#5661=DERIVED_UNIT_ELEMENT(#5683,1.);
#5662=DERIVED_UNIT_ELEMENT(#10021,-3.);
#5663=DERIVED_UNIT_ELEMENT(#5683,1.);
#5664=DERIVED_UNIT_ELEMENT(#10021,-3.);
#5665=DERIVED_UNIT_ELEMENT(#5683,1.);
#5666=DERIVED_UNIT_ELEMENT(#10021,-3.);
#5667=DERIVED_UNIT_ELEMENT(#5683,1.);
#5668=DERIVED_UNIT_ELEMENT(#10021,-3.);
#5669=DERIVED_UNIT_ELEMENT(#5683,1.);
#5670=DERIVED_UNIT_ELEMENT(#10021,-3.);
#5671=DERIVED_UNIT_ELEMENT(#5683,1.);
#5672=DERIVED_UNIT_ELEMENT(#10021,-3.);
#5673=DERIVED_UNIT_ELEMENT(#5683,1.);
#5674=DERIVED_UNIT_ELEMENT(#10021,-3.);
#5675=DERIVED_UNIT_ELEMENT(#5683,1.);
#5676=DERIVED_UNIT_ELEMENT(#10021,-3.);
#5677=DERIVED_UNIT_ELEMENT(#5683,1.);
#5678=DERIVED_UNIT_ELEMENT(#10021,-3.);
#5679=DERIVED_UNIT_ELEMENT(#5683,1.);
#5680=DERIVED_UNIT_ELEMENT(#10021,-3.);
#5681=DERIVED_UNIT_ELEMENT(#5683,1.);
#5682=DERIVED_UNIT_ELEMENT(#10021,-3.);
#5683=(
MASS_UNIT()
NAMED_UNIT(*)
SI_UNIT(.KILO.,.GRAM.)
);
#5684=DERIVED_UNIT((#5639,#5640));
#5685=DERIVED_UNIT((#5641,#5642));
#5686=DERIVED_UNIT((#5643,#5644));
#5687=DERIVED_UNIT((#5645,#5646));
#5688=DERIVED_UNIT((#5647,#5648));
#5689=DERIVED_UNIT((#5649,#5650));
#5690=DERIVED_UNIT((#5651,#5652));
#5691=DERIVED_UNIT((#5653,#5654));
#5692=DERIVED_UNIT((#5655,#5656));
#5693=DERIVED_UNIT((#5657,#5658));
#5694=DERIVED_UNIT((#5659,#5660));
#5695=DERIVED_UNIT((#5661,#5662));
#5696=DERIVED_UNIT((#5663,#5664));
#5697=DERIVED_UNIT((#5665,#5666));
#5698=DERIVED_UNIT((#5667,#5668));
#5699=DERIVED_UNIT((#5669,#5670));
#5700=DERIVED_UNIT((#5671,#5672));
#5701=DERIVED_UNIT((#5673,#5674));
#5702=DERIVED_UNIT((#5675,#5676));
#5703=DERIVED_UNIT((#5677,#5678));
#5704=DERIVED_UNIT((#5679,#5680));
#5705=DERIVED_UNIT((#5681,#5682));
#5706=MEASURE_REPRESENTATION_ITEM('density measure',
POSITIVE_RATIO_MEASURE(7850.),#5684);
#5707=MEASURE_REPRESENTATION_ITEM('density measure',
POSITIVE_RATIO_MEASURE(7850.),#5685);
#5708=MEASURE_REPRESENTATION_ITEM('density measure',
POSITIVE_RATIO_MEASURE(7850.),#5686);
#5709=MEASURE_REPRESENTATION_ITEM('density measure',
POSITIVE_RATIO_MEASURE(7850.),#5687);
#5710=MEASURE_REPRESENTATION_ITEM('density measure',
POSITIVE_RATIO_MEASURE(7850.),#5688);
#5711=MEASURE_REPRESENTATION_ITEM('density measure',
POSITIVE_RATIO_MEASURE(7850.),#5689);
#5712=MEASURE_REPRESENTATION_ITEM('density measure',
POSITIVE_RATIO_MEASURE(7850.),#5690);
#5713=MEASURE_REPRESENTATION_ITEM('density measure',
POSITIVE_RATIO_MEASURE(7850.),#5691);
#5714=MEASURE_REPRESENTATION_ITEM('density measure',
POSITIVE_RATIO_MEASURE(7850.),#5692);
#5715=MEASURE_REPRESENTATION_ITEM('density measure',
POSITIVE_RATIO_MEASURE(7850.),#5693);
#5716=MEASURE_REPRESENTATION_ITEM('density measure',
POSITIVE_RATIO_MEASURE(7850.),#5694);
#5717=MEASURE_REPRESENTATION_ITEM('density measure',
POSITIVE_RATIO_MEASURE(7850.),#5695);
#5718=MEASURE_REPRESENTATION_ITEM('density measure',
POSITIVE_RATIO_MEASURE(7850.),#5696);
#5719=MEASURE_REPRESENTATION_ITEM('density measure',
POSITIVE_RATIO_MEASURE(7850.),#5697);
#5720=MEASURE_REPRESENTATION_ITEM('density measure',
POSITIVE_RATIO_MEASURE(7850.),#5698);
#5721=MEASURE_REPRESENTATION_ITEM('density measure',
POSITIVE_RATIO_MEASURE(7850.),#5699);
#5722=MEASURE_REPRESENTATION_ITEM('density measure',
POSITIVE_RATIO_MEASURE(7850.),#5700);
#5723=MEASURE_REPRESENTATION_ITEM('density measure',
POSITIVE_RATIO_MEASURE(7850.),#5701);
#5724=MEASURE_REPRESENTATION_ITEM('density measure',
POSITIVE_RATIO_MEASURE(7850.),#5702);
#5725=MEASURE_REPRESENTATION_ITEM('density measure',
POSITIVE_RATIO_MEASURE(7850.),#5703);
#5726=MEASURE_REPRESENTATION_ITEM('density measure',
POSITIVE_RATIO_MEASURE(7850.),#5704);
#5727=MEASURE_REPRESENTATION_ITEM('density measure',
POSITIVE_RATIO_MEASURE(7850.),#5705);
#5728=PROPERTY_DEFINITION_REPRESENTATION(#5838,#5772);
#5729=PROPERTY_DEFINITION_REPRESENTATION(#5839,#5773);
#5730=PROPERTY_DEFINITION_REPRESENTATION(#5840,#5774);
#5731=PROPERTY_DEFINITION_REPRESENTATION(#5841,#5775);
#5732=PROPERTY_DEFINITION_REPRESENTATION(#5842,#5776);
#5733=PROPERTY_DEFINITION_REPRESENTATION(#5843,#5777);
#5734=PROPERTY_DEFINITION_REPRESENTATION(#5844,#5778);
#5735=PROPERTY_DEFINITION_REPRESENTATION(#5845,#5779);
#5736=PROPERTY_DEFINITION_REPRESENTATION(#5846,#5780);
#5737=PROPERTY_DEFINITION_REPRESENTATION(#5847,#5781);
#5738=PROPERTY_DEFINITION_REPRESENTATION(#5848,#5782);
#5739=PROPERTY_DEFINITION_REPRESENTATION(#5849,#5783);
#5740=PROPERTY_DEFINITION_REPRESENTATION(#5850,#5784);
#5741=PROPERTY_DEFINITION_REPRESENTATION(#5851,#5785);
#5742=PROPERTY_DEFINITION_REPRESENTATION(#5852,#5786);
#5743=PROPERTY_DEFINITION_REPRESENTATION(#5853,#5787);
#5744=PROPERTY_DEFINITION_REPRESENTATION(#5854,#5788);
#5745=PROPERTY_DEFINITION_REPRESENTATION(#5855,#5789);
#5746=PROPERTY_DEFINITION_REPRESENTATION(#5856,#5790);
#5747=PROPERTY_DEFINITION_REPRESENTATION(#5857,#5791);
#5748=PROPERTY_DEFINITION_REPRESENTATION(#5858,#5792);
#5749=PROPERTY_DEFINITION_REPRESENTATION(#5859,#5793);
#5750=PROPERTY_DEFINITION_REPRESENTATION(#5860,#5794);
#5751=PROPERTY_DEFINITION_REPRESENTATION(#5861,#5795);
#5752=PROPERTY_DEFINITION_REPRESENTATION(#5862,#5796);
#5753=PROPERTY_DEFINITION_REPRESENTATION(#5863,#5797);
#5754=PROPERTY_DEFINITION_REPRESENTATION(#5864,#5798);
#5755=PROPERTY_DEFINITION_REPRESENTATION(#5865,#5799);
#5756=PROPERTY_DEFINITION_REPRESENTATION(#5866,#5800);
#5757=PROPERTY_DEFINITION_REPRESENTATION(#5867,#5801);
#5758=PROPERTY_DEFINITION_REPRESENTATION(#5868,#5802);
#5759=PROPERTY_DEFINITION_REPRESENTATION(#5869,#5803);
#5760=PROPERTY_DEFINITION_REPRESENTATION(#5870,#5804);
#5761=PROPERTY_DEFINITION_REPRESENTATION(#5871,#5805);
#5762=PROPERTY_DEFINITION_REPRESENTATION(#5872,#5806);
#5763=PROPERTY_DEFINITION_REPRESENTATION(#5873,#5807);
#5764=PROPERTY_DEFINITION_REPRESENTATION(#5874,#5808);
#5765=PROPERTY_DEFINITION_REPRESENTATION(#5875,#5809);
#5766=PROPERTY_DEFINITION_REPRESENTATION(#5876,#5810);
#5767=PROPERTY_DEFINITION_REPRESENTATION(#5877,#5811);
#5768=PROPERTY_DEFINITION_REPRESENTATION(#5878,#5812);
#5769=PROPERTY_DEFINITION_REPRESENTATION(#5879,#5813);
#5770=PROPERTY_DEFINITION_REPRESENTATION(#5880,#5814);
#5771=PROPERTY_DEFINITION_REPRESENTATION(#5881,#5815);
#5772=REPRESENTATION('material name',(#5816),#9997);
#5773=REPRESENTATION('density',(#5706),#9997);
#5774=REPRESENTATION('material name',(#5817),#9998);
#5775=REPRESENTATION('density',(#5707),#9998);
#5776=REPRESENTATION('material name',(#5818),#9999);
#5777=REPRESENTATION('density',(#5708),#9999);
#5778=REPRESENTATION('material name',(#5819),#10000);
#5779=REPRESENTATION('density',(#5709),#10000);
#5780=REPRESENTATION('material name',(#5820),#10001);
#5781=REPRESENTATION('density',(#5710),#10001);
#5782=REPRESENTATION('material name',(#5821),#10002);
#5783=REPRESENTATION('density',(#5711),#10002);
#5784=REPRESENTATION('material name',(#5822),#10003);
#5785=REPRESENTATION('density',(#5712),#10003);
#5786=REPRESENTATION('material name',(#5823),#10004);
#5787=REPRESENTATION('density',(#5713),#10004);
#5788=REPRESENTATION('material name',(#5824),#10005);
#5789=REPRESENTATION('density',(#5714),#10005);
#5790=REPRESENTATION('material name',(#5825),#10006);
#5791=REPRESENTATION('density',(#5715),#10006);
#5792=REPRESENTATION('material name',(#5826),#10007);
#5793=REPRESENTATION('density',(#5716),#10007);
#5794=REPRESENTATION('material name',(#5827),#10008);
#5795=REPRESENTATION('density',(#5717),#10008);
#5796=REPRESENTATION('material name',(#5828),#10009);
#5797=REPRESENTATION('density',(#5718),#10009);
#5798=REPRESENTATION('material name',(#5829),#10010);
#5799=REPRESENTATION('density',(#5719),#10010);
#5800=REPRESENTATION('material name',(#5830),#10011);
#5801=REPRESENTATION('density',(#5720),#10011);
#5802=REPRESENTATION('material name',(#5831),#10012);
#5803=REPRESENTATION('density',(#5721),#10012);
#5804=REPRESENTATION('material name',(#5832),#10013);
#5805=REPRESENTATION('density',(#5722),#10013);
#5806=REPRESENTATION('material name',(#5833),#10014);
#5807=REPRESENTATION('density',(#5723),#10014);
#5808=REPRESENTATION('material name',(#5834),#10015);
#5809=REPRESENTATION('density',(#5724),#10015);
#5810=REPRESENTATION('material name',(#5835),#10016);
#5811=REPRESENTATION('density',(#5725),#10016);
#5812=REPRESENTATION('material name',(#5836),#10017);
#5813=REPRESENTATION('density',(#5726),#10017);
#5814=REPRESENTATION('material name',(#5837),#10018);
#5815=REPRESENTATION('density',(#5727),#10018);
#5816=DESCRIPTIVE_REPRESENTATION_ITEM('Steel','Steel');
#5817=DESCRIPTIVE_REPRESENTATION_ITEM('Steel','Steel');
#5818=DESCRIPTIVE_REPRESENTATION_ITEM('Steel','Steel');
#5819=DESCRIPTIVE_REPRESENTATION_ITEM('Steel','Steel');
#5820=DESCRIPTIVE_REPRESENTATION_ITEM('Steel','Steel');
#5821=DESCRIPTIVE_REPRESENTATION_ITEM('Steel','Steel');
#5822=DESCRIPTIVE_REPRESENTATION_ITEM('Steel','Steel');
#5823=DESCRIPTIVE_REPRESENTATION_ITEM('Steel','Steel');
#5824=DESCRIPTIVE_REPRESENTATION_ITEM('Steel','Steel');
#5825=DESCRIPTIVE_REPRESENTATION_ITEM('Steel','Steel');
#5826=DESCRIPTIVE_REPRESENTATION_ITEM('Steel','Steel');
#5827=DESCRIPTIVE_REPRESENTATION_ITEM('Steel','Steel');
#5828=DESCRIPTIVE_REPRESENTATION_ITEM('Steel','Steel');
#5829=DESCRIPTIVE_REPRESENTATION_ITEM('Steel','Steel');
#5830=DESCRIPTIVE_REPRESENTATION_ITEM('Steel','Steel');
#5831=DESCRIPTIVE_REPRESENTATION_ITEM('Steel','Steel');
#5832=DESCRIPTIVE_REPRESENTATION_ITEM('Steel','Steel');
#5833=DESCRIPTIVE_REPRESENTATION_ITEM('Steel','Steel');
#5834=DESCRIPTIVE_REPRESENTATION_ITEM('Steel','Steel');
#5835=DESCRIPTIVE_REPRESENTATION_ITEM('Steel','Steel');
#5836=DESCRIPTIVE_REPRESENTATION_ITEM('Steel','Steel');
#5837=DESCRIPTIVE_REPRESENTATION_ITEM('Steel','Steel');
#5838=PROPERTY_DEFINITION('material property','material name',#10192);
#5839=PROPERTY_DEFINITION('material property','density of part',#10192);
#5840=PROPERTY_DEFINITION('material property','material name',#10193);
#5841=PROPERTY_DEFINITION('material property','density of part',#10193);
#5842=PROPERTY_DEFINITION('material property','material name',#10194);
#5843=PROPERTY_DEFINITION('material property','density of part',#10194);
#5844=PROPERTY_DEFINITION('material property','material name',#10195);
#5845=PROPERTY_DEFINITION('material property','density of part',#10195);
#5846=PROPERTY_DEFINITION('material property','material name',#10196);
#5847=PROPERTY_DEFINITION('material property','density of part',#10196);
#5848=PROPERTY_DEFINITION('material property','material name',#10197);
#5849=PROPERTY_DEFINITION('material property','density of part',#10197);
#5850=PROPERTY_DEFINITION('material property','material name',#10198);
#5851=PROPERTY_DEFINITION('material property','density of part',#10198);
#5852=PROPERTY_DEFINITION('material property','material name',#10199);
#5853=PROPERTY_DEFINITION('material property','density of part',#10199);
#5854=PROPERTY_DEFINITION('material property','material name',#10200);
#5855=PROPERTY_DEFINITION('material property','density of part',#10200);
#5856=PROPERTY_DEFINITION('material property','material name',#10201);
#5857=PROPERTY_DEFINITION('material property','density of part',#10201);
#5858=PROPERTY_DEFINITION('material property','material name',#10202);
#5859=PROPERTY_DEFINITION('material property','density of part',#10202);
#5860=PROPERTY_DEFINITION('material property','material name',#10203);
#5861=PROPERTY_DEFINITION('material property','density of part',#10203);
#5862=PROPERTY_DEFINITION('material property','material name',#10204);
#5863=PROPERTY_DEFINITION('material property','density of part',#10204);
#5864=PROPERTY_DEFINITION('material property','material name',#10205);
#5865=PROPERTY_DEFINITION('material property','density of part',#10205);
#5866=PROPERTY_DEFINITION('material property','material name',#10206);
#5867=PROPERTY_DEFINITION('material property','density of part',#10206);
#5868=PROPERTY_DEFINITION('material property','material name',#10207);
#5869=PROPERTY_DEFINITION('material property','density of part',#10207);
#5870=PROPERTY_DEFINITION('material property','material name',#10208);
#5871=PROPERTY_DEFINITION('material property','density of part',#10208);
#5872=PROPERTY_DEFINITION('material property','material name',#10209);
#5873=PROPERTY_DEFINITION('material property','density of part',#10209);
#5874=PROPERTY_DEFINITION('material property','material name',#10210);
#5875=PROPERTY_DEFINITION('material property','density of part',#10210);
#5876=PROPERTY_DEFINITION('material property','material name',#10211);
#5877=PROPERTY_DEFINITION('material property','density of part',#10211);
#5878=PROPERTY_DEFINITION('material property','material name',#10212);
#5879=PROPERTY_DEFINITION('material property','density of part',#10212);
#5880=PROPERTY_DEFINITION('material property','material name',#10213);
#5881=PROPERTY_DEFINITION('material property','density of part',#10213);
#5882=AXIS2_PLACEMENT_3D('',#8058,#6426,#6427);
#5883=AXIS2_PLACEMENT_3D('',#8059,#6428,#6429);
#5884=AXIS2_PLACEMENT_3D('',#8060,#6430,#6431);
#5885=AXIS2_PLACEMENT_3D('',#8062,#6432,#6433);
#5886=AXIS2_PLACEMENT_3D('',#8065,#6435,#6436);
#5887=AXIS2_PLACEMENT_3D('',#8066,#6437,#6438);
#5888=AXIS2_PLACEMENT_3D('',#8068,#6439,#6440);
#5889=AXIS2_PLACEMENT_3D('',#8071,#6442,#6443);
#5890=AXIS2_PLACEMENT_3D('',#8072,#6444,#6445);
#5891=AXIS2_PLACEMENT_3D('',#8073,#6446,#6447);
#5892=AXIS2_PLACEMENT_3D('',#8074,#6448,#6449);
#5893=AXIS2_PLACEMENT_3D('',#8075,#6450,#6451);
#5894=AXIS2_PLACEMENT_3D('',#8077,#6452,#6453);
#5895=AXIS2_PLACEMENT_3D('',#8080,#6455,#6456);
#5896=AXIS2_PLACEMENT_3D('',#8081,#6457,#6458);
#5897=AXIS2_PLACEMENT_3D('',#8083,#6459,#6460);
#5898=AXIS2_PLACEMENT_3D('',#8086,#6462,#6463);
#5899=AXIS2_PLACEMENT_3D('',#8087,#6464,#6465);
#5900=AXIS2_PLACEMENT_3D('',#8088,#6466,#6467);
#5901=AXIS2_PLACEMENT_3D('',#8089,#6468,#6469);
#5902=AXIS2_PLACEMENT_3D('',#8090,#6470,#6471);
#5903=AXIS2_PLACEMENT_3D('',#8092,#6472,#6473);
#5904=AXIS2_PLACEMENT_3D('',#8095,#6475,#6476);
#5905=AXIS2_PLACEMENT_3D('',#8096,#6477,#6478);
#5906=AXIS2_PLACEMENT_3D('',#8098,#6479,#6480);
#5907=AXIS2_PLACEMENT_3D('',#8101,#6482,#6483);
#5908=AXIS2_PLACEMENT_3D('',#8102,#6484,#6485);
#5909=AXIS2_PLACEMENT_3D('',#8103,#6486,#6487);
#5910=AXIS2_PLACEMENT_3D('',#8104,#6488,#6489);
#5911=AXIS2_PLACEMENT_3D('',#8105,#6490,#6491);
#5912=AXIS2_PLACEMENT_3D('',#8107,#6492,#6493);
#5913=AXIS2_PLACEMENT_3D('',#8110,#6495,#6496);
#5914=AXIS2_PLACEMENT_3D('',#8111,#6497,#6498);
#5915=AXIS2_PLACEMENT_3D('',#8113,#6499,#6500);
#5916=AXIS2_PLACEMENT_3D('',#8116,#6502,#6503);
#5917=AXIS2_PLACEMENT_3D('',#8117,#6504,#6505);
#5918=AXIS2_PLACEMENT_3D('',#8118,#6506,#6507);
#5919=AXIS2_PLACEMENT_3D('',#8119,#6508,#6509);
#5920=AXIS2_PLACEMENT_3D('',#8120,#6510,#6511);
#5921=AXIS2_PLACEMENT_3D('',#8122,#6512,#6513);
#5922=AXIS2_PLACEMENT_3D('',#8125,#6515,#6516);
#5923=AXIS2_PLACEMENT_3D('',#8126,#6517,#6518);
#5924=AXIS2_PLACEMENT_3D('',#8128,#6519,#6520);
#5925=AXIS2_PLACEMENT_3D('',#8131,#6522,#6523);
#5926=AXIS2_PLACEMENT_3D('',#8132,#6524,#6525);
#5927=AXIS2_PLACEMENT_3D('',#8133,#6526,#6527);
#5928=AXIS2_PLACEMENT_3D('',#8134,#6528,#6529);
#5929=AXIS2_PLACEMENT_3D('',#8135,#6530,#6531);
#5930=AXIS2_PLACEMENT_3D('',#8137,#6532,#6533);
#5931=AXIS2_PLACEMENT_3D('',#8140,#6535,#6536);
#5932=AXIS2_PLACEMENT_3D('',#8141,#6537,#6538);
#5933=AXIS2_PLACEMENT_3D('',#8143,#6539,#6540);
#5934=AXIS2_PLACEMENT_3D('',#8146,#6542,#6543);
#5935=AXIS2_PLACEMENT_3D('',#8147,#6544,#6545);
#5936=AXIS2_PLACEMENT_3D('',#8148,#6546,#6547);
#5937=AXIS2_PLACEMENT_3D('',#8149,#6548,#6549);
#5938=AXIS2_PLACEMENT_3D('',#8150,#6550,#6551);
#5939=AXIS2_PLACEMENT_3D('',#8152,#6552,#6553);
#5940=AXIS2_PLACEMENT_3D('',#8155,#6555,#6556);
#5941=AXIS2_PLACEMENT_3D('',#8156,#6557,#6558);
#5942=AXIS2_PLACEMENT_3D('',#8158,#6559,#6560);
#5943=AXIS2_PLACEMENT_3D('',#8161,#6562,#6563);
#5944=AXIS2_PLACEMENT_3D('',#8162,#6564,#6565);
#5945=AXIS2_PLACEMENT_3D('',#8163,#6566,#6567);
#5946=AXIS2_PLACEMENT_3D('',#8164,#6568,#6569);
#5947=AXIS2_PLACEMENT_3D('',#8165,#6570,#6571);
#5948=AXIS2_PLACEMENT_3D('',#8167,#6572,#6573);
#5949=AXIS2_PLACEMENT_3D('',#8170,#6575,#6576);
#5950=AXIS2_PLACEMENT_3D('',#8171,#6577,#6578);
#5951=AXIS2_PLACEMENT_3D('',#8173,#6579,#6580);
#5952=AXIS2_PLACEMENT_3D('',#8176,#6582,#6583);
#5953=AXIS2_PLACEMENT_3D('',#8177,#6584,#6585);
#5954=AXIS2_PLACEMENT_3D('',#8178,#6586,#6587);
#5955=AXIS2_PLACEMENT_3D('',#8179,#6588,#6589);
#5956=AXIS2_PLACEMENT_3D('',#8180,#6590,#6591);
#5957=AXIS2_PLACEMENT_3D('',#8182,#6592,#6593);
#5958=AXIS2_PLACEMENT_3D('',#8185,#6595,#6596);
#5959=AXIS2_PLACEMENT_3D('',#8186,#6597,#6598);
#5960=AXIS2_PLACEMENT_3D('',#8188,#6599,#6600);
#5961=AXIS2_PLACEMENT_3D('',#8189,#6601,#6602);
#5962=AXIS2_PLACEMENT_3D('',#8191,#6603,#6604);
#5963=AXIS2_PLACEMENT_3D('',#8194,#6606,#6607);
#5964=AXIS2_PLACEMENT_3D('',#8195,#6608,#6609);
#5965=AXIS2_PLACEMENT_3D('',#8197,#6610,#6611);
#5966=AXIS2_PLACEMENT_3D('',#8198,#6612,#6613);
#5967=AXIS2_PLACEMENT_3D('',#8200,#6614,#6615);
#5968=AXIS2_PLACEMENT_3D('',#8203,#6617,#6618);
#5969=AXIS2_PLACEMENT_3D('',#8204,#6619,#6620);
#5970=AXIS2_PLACEMENT_3D('',#8206,#6621,#6622);
#5971=AXIS2_PLACEMENT_3D('',#8207,#6623,#6624);
#5972=AXIS2_PLACEMENT_3D('',#8209,#6625,#6626);
#5973=AXIS2_PLACEMENT_3D('',#8212,#6628,#6629);
#5974=AXIS2_PLACEMENT_3D('',#8213,#6630,#6631);
#5975=AXIS2_PLACEMENT_3D('',#8215,#6632,#6633);
#5976=AXIS2_PLACEMENT_3D('',#8216,#6634,#6635);
#5977=AXIS2_PLACEMENT_3D('',#8218,#6636,#6637);
#5978=AXIS2_PLACEMENT_3D('',#8220,#6639,#6640);
#5979=AXIS2_PLACEMENT_3D('',#8222,#6641,#6642);
#5980=AXIS2_PLACEMENT_3D('',#8224,#6644,#6645);
#5981=AXIS2_PLACEMENT_3D('',#8226,#6646,#6647);
#5982=AXIS2_PLACEMENT_3D('',#8228,#6649,#6650);
#5983=AXIS2_PLACEMENT_3D('',#8230,#6651,#6652);
#5984=AXIS2_PLACEMENT_3D('',#8232,#6654,#6655);
#5985=AXIS2_PLACEMENT_3D('',#8241,#6660,#6661);
#5986=AXIS2_PLACEMENT_3D('',#8247,#6665,#6666);
#5987=AXIS2_PLACEMENT_3D('',#8253,#6670,#6671);
#5988=AXIS2_PLACEMENT_3D('',#8256,#6674,#6675);
#5989=AXIS2_PLACEMENT_3D('',#8257,#6676,#6677);
#5990=AXIS2_PLACEMENT_3D('',#8258,#6678,#6679);
#5991=AXIS2_PLACEMENT_3D('',#8259,#6680,#6681);
#5992=AXIS2_PLACEMENT_3D('',#8261,#6682,#6683);
#5993=AXIS2_PLACEMENT_3D('',#8264,#6685,#6686);
#5994=AXIS2_PLACEMENT_3D('',#8265,#6687,#6688);
#5995=AXIS2_PLACEMENT_3D('',#8267,#6689,#6690);
#5996=AXIS2_PLACEMENT_3D('',#8270,#6692,#6693);
#5997=AXIS2_PLACEMENT_3D('',#8271,#6694,#6695);
#5998=AXIS2_PLACEMENT_3D('',#8273,#6696,#6697);
#5999=AXIS2_PLACEMENT_3D('',#8276,#6699,#6700);
#6000=AXIS2_PLACEMENT_3D('',#8277,#6701,#6702);
#6001=AXIS2_PLACEMENT_3D('',#8279,#6703,#6704);
#6002=AXIS2_PLACEMENT_3D('',#8282,#6706,#6707);
#6003=AXIS2_PLACEMENT_3D('',#8283,#6708,#6709);
#6004=AXIS2_PLACEMENT_3D('',#8292,#6714,#6715);
#6005=AXIS2_PLACEMENT_3D('',#8298,#6719,#6720);
#6006=AXIS2_PLACEMENT_3D('',#8304,#6724,#6725);
#6007=AXIS2_PLACEMENT_3D('',#8322,#6735,#6736);
#6008=AXIS2_PLACEMENT_3D('',#8328,#6740,#6741);
#6009=AXIS2_PLACEMENT_3D('',#8330,#6743,#6744);
#6010=AXIS2_PLACEMENT_3D('',#8334,#6747,#6748);
#6011=AXIS2_PLACEMENT_3D('',#8340,#6752,#6753);
#6012=AXIS2_PLACEMENT_3D('',#8344,#6756,#6757);
#6013=AXIS2_PLACEMENT_3D('',#8346,#6759,#6760);
#6014=AXIS2_PLACEMENT_3D('',#8350,#6763,#6764);
#6015=AXIS2_PLACEMENT_3D('',#8354,#6767,#6768);
#6016=AXIS2_PLACEMENT_3D('',#8356,#6770,#6771);
#6017=AXIS2_PLACEMENT_3D('',#8357,#6772,#6773);
#6018=AXIS2_PLACEMENT_3D('',#8358,#6774,#6775);
#6019=AXIS2_PLACEMENT_3D('',#8360,#6776,#6777);
#6020=AXIS2_PLACEMENT_3D('',#8363,#6779,#6780);
#6021=AXIS2_PLACEMENT_3D('',#8364,#6781,#6782);
#6022=AXIS2_PLACEMENT_3D('',#8366,#6783,#6784);
#6023=AXIS2_PLACEMENT_3D('',#8369,#6786,#6787);
#6024=AXIS2_PLACEMENT_3D('',#8370,#6788,#6789);
#6025=AXIS2_PLACEMENT_3D('',#8372,#6790,#6791);
#6026=AXIS2_PLACEMENT_3D('',#8375,#6793,#6794);
#6027=AXIS2_PLACEMENT_3D('',#8376,#6795,#6796);
#6028=AXIS2_PLACEMENT_3D('',#8385,#6801,#6802);
#6029=AXIS2_PLACEMENT_3D('',#8391,#6806,#6807);
#6030=AXIS2_PLACEMENT_3D('',#8397,#6811,#6812);
#6031=AXIS2_PLACEMENT_3D('',#8403,#6816,#6817);
#6032=AXIS2_PLACEMENT_3D('',#8409,#6821,#6822);
#6033=AXIS2_PLACEMENT_3D('',#8412,#6825,#6826);
#6034=AXIS2_PLACEMENT_3D('',#8413,#6827,#6828);
#6035=AXIS2_PLACEMENT_3D('',#8414,#6829,#6830);
#6036=AXIS2_PLACEMENT_3D('',#8415,#6831,#6832);
#6037=AXIS2_PLACEMENT_3D('',#8417,#6833,#6834);
#6038=AXIS2_PLACEMENT_3D('',#8420,#6836,#6837);
#6039=AXIS2_PLACEMENT_3D('',#8421,#6838,#6839);
#6040=AXIS2_PLACEMENT_3D('',#8423,#6840,#6841);
#6041=AXIS2_PLACEMENT_3D('',#8426,#6843,#6844);
#6042=AXIS2_PLACEMENT_3D('',#8427,#6845,#6846);
#6043=AXIS2_PLACEMENT_3D('',#8429,#6847,#6848);
#6044=AXIS2_PLACEMENT_3D('',#8432,#6850,#6851);
#6045=AXIS2_PLACEMENT_3D('',#8433,#6852,#6853);
#6046=AXIS2_PLACEMENT_3D('',#8442,#6858,#6859);
#6047=AXIS2_PLACEMENT_3D('',#8448,#6863,#6864);
#6048=AXIS2_PLACEMENT_3D('',#8454,#6868,#6869);
#6049=AXIS2_PLACEMENT_3D('',#8460,#6873,#6874);
#6050=AXIS2_PLACEMENT_3D('',#8466,#6878,#6879);
#6051=AXIS2_PLACEMENT_3D('',#8469,#6882,#6883);
#6052=AXIS2_PLACEMENT_3D('',#8470,#6884,#6885);
#6053=AXIS2_PLACEMENT_3D('',#8471,#6886,#6887);
#6054=AXIS2_PLACEMENT_3D('',#8472,#6888,#6889);
#6055=AXIS2_PLACEMENT_3D('',#8474,#6890,#6891);
#6056=AXIS2_PLACEMENT_3D('',#8477,#6893,#6894);
#6057=AXIS2_PLACEMENT_3D('',#8478,#6895,#6896);
#6058=AXIS2_PLACEMENT_3D('',#8480,#6897,#6898);
#6059=AXIS2_PLACEMENT_3D('',#8483,#6900,#6901);
#6060=AXIS2_PLACEMENT_3D('',#8484,#6902,#6903);
#6061=AXIS2_PLACEMENT_3D('',#8493,#6908,#6909);
#6062=AXIS2_PLACEMENT_3D('',#8499,#6913,#6914);
#6063=AXIS2_PLACEMENT_3D('',#8505,#6918,#6919);
#6064=AXIS2_PLACEMENT_3D('',#8508,#6922,#6923);
#6065=AXIS2_PLACEMENT_3D('',#8509,#6924,#6925);
#6066=AXIS2_PLACEMENT_3D('',#8510,#6926,#6927);
#6067=AXIS2_PLACEMENT_3D('',#8511,#6928,#6929);
#6068=AXIS2_PLACEMENT_3D('',#8513,#6930,#6931);
#6069=AXIS2_PLACEMENT_3D('',#8544,#6934,#6935);
#6070=AXIS2_PLACEMENT_3D('',#8616,#6936,#6937);
#6071=AXIS2_PLACEMENT_3D('',#8618,#6938,#6939);
#6072=AXIS2_PLACEMENT_3D('',#8649,#6942,#6943);
#6073=AXIS2_PLACEMENT_3D('',#8721,#6944,#6945);
#6074=AXIS2_PLACEMENT_3D('',#8723,#6947,#6948);
#6075=AXIS2_PLACEMENT_3D('',#8771,#6950,#6951);
#6076=AXIS2_PLACEMENT_3D('',#8773,#6952,#6953);
#6077=AXIS2_PLACEMENT_3D('',#8801,#6956,#6957);
#6078=AXIS2_PLACEMENT_3D('',#8827,#6958,#6959);
#6079=AXIS2_PLACEMENT_3D('',#8829,#6960,#6961);
#6080=AXIS2_PLACEMENT_3D('',#8857,#6964,#6965);
#6081=AXIS2_PLACEMENT_3D('',#8929,#6966,#6967);
#6082=AXIS2_PLACEMENT_3D('',#8931,#6969,#6970);
#6083=AXIS2_PLACEMENT_3D('',#8933,#6971,#6972);
#6084=AXIS2_PLACEMENT_3D('',#8935,#6974,#6975);
#6085=AXIS2_PLACEMENT_3D('',#8944,#6980,#6981);
#6086=AXIS2_PLACEMENT_3D('',#8950,#6985,#6986);
#6087=AXIS2_PLACEMENT_3D('',#8956,#6990,#6991);
#6088=AXIS2_PLACEMENT_3D('',#8962,#6995,#6996);
#6089=AXIS2_PLACEMENT_3D('',#8968,#7000,#7001);
#6090=AXIS2_PLACEMENT_3D('',#8974,#7005,#7006);
#6091=AXIS2_PLACEMENT_3D('',#8980,#7010,#7011);
#6092=AXIS2_PLACEMENT_3D('',#8986,#7015,#7016);
#6093=AXIS2_PLACEMENT_3D('',#8992,#7020,#7021);
#6094=AXIS2_PLACEMENT_3D('',#9001,#7026,#7027);
#6095=AXIS2_PLACEMENT_3D('',#9007,#7031,#7032);
#6096=AXIS2_PLACEMENT_3D('',#9013,#7036,#7037);
#6097=AXIS2_PLACEMENT_3D('',#9019,#7041,#7042);
#6098=AXIS2_PLACEMENT_3D('',#9025,#7046,#7047);
#6099=AXIS2_PLACEMENT_3D('',#9031,#7051,#7052);
#6100=AXIS2_PLACEMENT_3D('',#9037,#7056,#7057);
#6101=AXIS2_PLACEMENT_3D('',#9043,#7061,#7062);
#6102=AXIS2_PLACEMENT_3D('',#9049,#7066,#7067);
#6103=AXIS2_PLACEMENT_3D('',#9058,#7072,#7073);
#6104=AXIS2_PLACEMENT_3D('',#9064,#7077,#7078);
#6105=AXIS2_PLACEMENT_3D('',#9070,#7082,#7083);
#6106=AXIS2_PLACEMENT_3D('',#9076,#7087,#7088);
#6107=AXIS2_PLACEMENT_3D('',#9082,#7092,#7093);
#6108=AXIS2_PLACEMENT_3D('',#9088,#7097,#7098);
#6109=AXIS2_PLACEMENT_3D('',#9094,#7102,#7103);
#6110=AXIS2_PLACEMENT_3D('',#9100,#7107,#7108);
#6111=AXIS2_PLACEMENT_3D('',#9106,#7112,#7113);
#6112=AXIS2_PLACEMENT_3D('',#9115,#7118,#7119);
#6113=AXIS2_PLACEMENT_3D('',#9121,#7123,#7124);
#6114=AXIS2_PLACEMENT_3D('',#9127,#7128,#7129);
#6115=AXIS2_PLACEMENT_3D('',#9133,#7133,#7134);
#6116=AXIS2_PLACEMENT_3D('',#9139,#7138,#7139);
#6117=AXIS2_PLACEMENT_3D('',#9145,#7143,#7144);
#6118=AXIS2_PLACEMENT_3D('',#9151,#7148,#7149);
#6119=AXIS2_PLACEMENT_3D('',#9157,#7153,#7154);
#6120=AXIS2_PLACEMENT_3D('',#9163,#7158,#7159);
#6121=AXIS2_PLACEMENT_3D('',#9166,#7161,#7162);
#6122=AXIS2_PLACEMENT_3D('',#9167,#7163,#7164);
#6123=AXIS2_PLACEMENT_3D('',#9173,#7168,#7169);
#6124=AXIS2_PLACEMENT_3D('',#9179,#7173,#7174);
#6125=AXIS2_PLACEMENT_3D('',#9182,#7177,#7178);
#6126=AXIS2_PLACEMENT_3D('',#9188,#7182,#7183);
#6127=AXIS2_PLACEMENT_3D('',#9191,#7186,#7187);
#6128=AXIS2_PLACEMENT_3D('',#9197,#7191,#7192);
#6129=AXIS2_PLACEMENT_3D('',#9200,#7195,#7196);
#6130=AXIS2_PLACEMENT_3D('',#9203,#7199,#7200);
#6131=AXIS2_PLACEMENT_3D('',#9204,#7201,#7202);
#6132=AXIS2_PLACEMENT_3D('',#9205,#7203,#7204);
#6133=AXIS2_PLACEMENT_3D('',#9206,#7205,#7206);
#6134=AXIS2_PLACEMENT_3D('',#9296,#7251,#7252);
#6135=AXIS2_PLACEMENT_3D('',#9297,#7253,#7254);
#6136=AXIS2_PLACEMENT_3D('',#9303,#7258,#7259);
#6137=AXIS2_PLACEMENT_3D('',#9307,#7262,#7263);
#6138=AXIS2_PLACEMENT_3D('',#9311,#7266,#7267);
#6139=AXIS2_PLACEMENT_3D('',#9315,#7270,#7271);
#6140=AXIS2_PLACEMENT_3D('',#9319,#7274,#7275);
#6141=AXIS2_PLACEMENT_3D('',#9323,#7278,#7279);
#6142=AXIS2_PLACEMENT_3D('',#9327,#7282,#7283);
#6143=AXIS2_PLACEMENT_3D('',#9331,#7286,#7287);
#6144=AXIS2_PLACEMENT_3D('',#9335,#7290,#7291);
#6145=AXIS2_PLACEMENT_3D('',#9339,#7294,#7295);
#6146=AXIS2_PLACEMENT_3D('',#9343,#7298,#7299);
#6147=AXIS2_PLACEMENT_3D('',#9347,#7302,#7303);
#6148=AXIS2_PLACEMENT_3D('',#9351,#7306,#7307);
#6149=AXIS2_PLACEMENT_3D('',#9355,#7310,#7311);
#6150=AXIS2_PLACEMENT_3D('',#9359,#7314,#7315);
#6151=AXIS2_PLACEMENT_3D('',#9363,#7318,#7319);
#6152=AXIS2_PLACEMENT_3D('',#9367,#7322,#7323);
#6153=AXIS2_PLACEMENT_3D('',#9371,#7326,#7327);
#6154=AXIS2_PLACEMENT_3D('',#9375,#7330,#7331);
#6155=AXIS2_PLACEMENT_3D('',#9379,#7334,#7335);
#6156=AXIS2_PLACEMENT_3D('',#9383,#7338,#7339);
#6157=AXIS2_PLACEMENT_3D('',#9387,#7342,#7343);
#6158=AXIS2_PLACEMENT_3D('',#9393,#7347,#7348);
#6159=AXIS2_PLACEMENT_3D('',#9397,#7351,#7352);
#6160=AXIS2_PLACEMENT_3D('',#9401,#7355,#7356);
#6161=AXIS2_PLACEMENT_3D('',#9405,#7359,#7360);
#6162=AXIS2_PLACEMENT_3D('',#9409,#7363,#7364);
#6163=AXIS2_PLACEMENT_3D('',#9413,#7367,#7368);
#6164=AXIS2_PLACEMENT_3D('',#9417,#7371,#7372);
#6165=AXIS2_PLACEMENT_3D('',#9421,#7375,#7376);
#6166=AXIS2_PLACEMENT_3D('',#9425,#7379,#7380);
#6167=AXIS2_PLACEMENT_3D('',#9429,#7383,#7384);
#6168=AXIS2_PLACEMENT_3D('',#9433,#7387,#7388);
#6169=AXIS2_PLACEMENT_3D('',#9437,#7391,#7392);
#6170=AXIS2_PLACEMENT_3D('',#9441,#7395,#7396);
#6171=AXIS2_PLACEMENT_3D('',#9445,#7399,#7400);
#6172=AXIS2_PLACEMENT_3D('',#9449,#7403,#7404);
#6173=AXIS2_PLACEMENT_3D('',#9453,#7407,#7408);
#6174=AXIS2_PLACEMENT_3D('',#9457,#7411,#7412);
#6175=AXIS2_PLACEMENT_3D('',#9461,#7415,#7416);
#6176=AXIS2_PLACEMENT_3D('',#9463,#7417,#7418);
#6177=AXIS2_PLACEMENT_3D('',#9465,#7420,#7421);
#6178=AXIS2_PLACEMENT_3D('',#9469,#7424,#7425);
#6179=AXIS2_PLACEMENT_3D('',#9473,#7428,#7429);
#6180=AXIS2_PLACEMENT_3D('',#9475,#7431,#7432);
#6181=AXIS2_PLACEMENT_3D('',#9477,#7434,#7435);
#6182=AXIS2_PLACEMENT_3D('',#9478,#7436,#7437);
#6183=AXIS2_PLACEMENT_3D('',#9479,#7438,#7439);
#6184=AXIS2_PLACEMENT_3D('',#9488,#7444,#7445);
#6185=AXIS2_PLACEMENT_3D('',#9494,#7449,#7450);
#6186=AXIS2_PLACEMENT_3D('',#9500,#7454,#7455);
#6187=AXIS2_PLACEMENT_3D('',#9506,#7459,#7460);
#6188=AXIS2_PLACEMENT_3D('',#9512,#7464,#7465);
#6189=AXIS2_PLACEMENT_3D('',#9515,#7468,#7469);
#6190=AXIS2_PLACEMENT_3D('',#9516,#7470,#7471);
#6191=AXIS2_PLACEMENT_3D('',#9517,#7472,#7473);
#6192=AXIS2_PLACEMENT_3D('',#9519,#7474,#7475);
#6193=AXIS2_PLACEMENT_3D('',#9521,#7476,#7477);
#6194=AXIS2_PLACEMENT_3D('',#9522,#7478,#7479);
#6195=AXIS2_PLACEMENT_3D('',#9525,#7481,#7482);
#6196=AXIS2_PLACEMENT_3D('',#9526,#7483,#7484);
#6197=AXIS2_PLACEMENT_3D('',#9527,#7485,#7486);
#6198=AXIS2_PLACEMENT_3D('',#9529,#7487,#7488);
#6199=AXIS2_PLACEMENT_3D('',#9530,#7489,#7490);
#6200=AXIS2_PLACEMENT_3D('',#9532,#7491,#7492);
#6201=AXIS2_PLACEMENT_3D('',#9534,#7494,#7495);
#6202=AXIS2_PLACEMENT_3D('',#9536,#7496,#7497);
#6203=AXIS2_PLACEMENT_3D('',#9538,#7499,#7500);
#6204=AXIS2_PLACEMENT_3D('',#9540,#7501,#7502);
#6205=AXIS2_PLACEMENT_3D('',#9542,#7504,#7505);
#6206=AXIS2_PLACEMENT_3D('',#9544,#7506,#7507);
#6207=AXIS2_PLACEMENT_3D('',#9545,#7508,#7509);
#6208=AXIS2_PLACEMENT_3D('',#9547,#7510,#7511);
#6209=AXIS2_PLACEMENT_3D('',#9549,#7513,#7514);
#6210=AXIS2_PLACEMENT_3D('',#9551,#7516,#7517);
#6211=AXIS2_PLACEMENT_3D('',#9552,#7518,#7519);
#6212=AXIS2_PLACEMENT_3D('',#9554,#7520,#7521);
#6213=AXIS2_PLACEMENT_3D('',#9555,#7522,#7523);
#6214=AXIS2_PLACEMENT_3D('',#9557,#7524,#7525);
#6215=AXIS2_PLACEMENT_3D('',#9559,#7527,#7528);
#6216=AXIS2_PLACEMENT_3D('',#9561,#7529,#7530);
#6217=AXIS2_PLACEMENT_3D('',#9563,#7532,#7533);
#6218=AXIS2_PLACEMENT_3D('',#9565,#7534,#7535);
#6219=AXIS2_PLACEMENT_3D('',#9567,#7537,#7538);
#6220=AXIS2_PLACEMENT_3D('',#9569,#7539,#7540);
#6221=AXIS2_PLACEMENT_3D('',#9570,#7541,#7542);
#6222=AXIS2_PLACEMENT_3D('',#9572,#7543,#7544);
#6223=AXIS2_PLACEMENT_3D('',#9574,#7546,#7547);
#6224=AXIS2_PLACEMENT_3D('',#9576,#7548,#7549);
#6225=AXIS2_PLACEMENT_3D('',#9578,#7551,#7552);
#6226=AXIS2_PLACEMENT_3D('',#9580,#7553,#7554);
#6227=AXIS2_PLACEMENT_3D('',#9582,#7556,#7557);
#6228=AXIS2_PLACEMENT_3D('',#9583,#7558,#7559);
#6229=AXIS2_PLACEMENT_3D('',#9592,#7564,#7565);
#6230=AXIS2_PLACEMENT_3D('',#9598,#7569,#7570);
#6231=AXIS2_PLACEMENT_3D('',#9604,#7574,#7575);
#6232=AXIS2_PLACEMENT_3D('',#9610,#7579,#7580);
#6233=AXIS2_PLACEMENT_3D('',#9616,#7584,#7585);
#6234=AXIS2_PLACEMENT_3D('',#9619,#7588,#7589);
#6235=AXIS2_PLACEMENT_3D('',#9620,#7590,#7591);
#6236=AXIS2_PLACEMENT_3D('',#9621,#7592,#7593);
#6237=AXIS2_PLACEMENT_3D('',#9622,#7594,#7595);
#6238=AXIS2_PLACEMENT_3D('',#9631,#7600,#7601);
#6239=AXIS2_PLACEMENT_3D('',#9637,#7605,#7606);
#6240=AXIS2_PLACEMENT_3D('',#9644,#7610,#7611);
#6241=AXIS2_PLACEMENT_3D('',#9645,#7612,#7613);
#6242=AXIS2_PLACEMENT_3D('',#9659,#7621,#7622);
#6243=AXIS2_PLACEMENT_3D('',#9663,#7625,#7626);
#6244=AXIS2_PLACEMENT_3D('',#9667,#7629,#7630);
#6245=AXIS2_PLACEMENT_3D('',#9677,#7636,#7637);
#6246=AXIS2_PLACEMENT_3D('',#9679,#7639,#7640);
#6247=AXIS2_PLACEMENT_3D('',#9683,#7642,#7643);
#6248=AXIS2_PLACEMENT_3D('',#9685,#7645,#7646);
#6249=AXIS2_PLACEMENT_3D('',#9687,#7647,#7648);
#6250=AXIS2_PLACEMENT_3D('',#9690,#7650,#7651);
#6251=AXIS2_PLACEMENT_3D('',#9692,#7652,#7653);
#6252=AXIS2_PLACEMENT_3D('',#9693,#7654,#7655);
#6253=AXIS2_PLACEMENT_3D('',#9694,#7656,#7657);
#6254=AXIS2_PLACEMENT_3D('',#9696,#7659,#7660);
#6255=AXIS2_PLACEMENT_3D('',#9698,#7662,#7663);
#6256=AXIS2_PLACEMENT_3D('',#9700,#7665,#7666);
#6257=AXIS2_PLACEMENT_3D('',#9701,#7667,#7668);
#6258=AXIS2_PLACEMENT_3D('',#9702,#7669,#7670);
#6259=AXIS2_PLACEMENT_3D('',#9704,#7671,#7672);
#6260=AXIS2_PLACEMENT_3D('',#9707,#7674,#7675);
#6261=AXIS2_PLACEMENT_3D('',#9708,#7676,#7677);
#6262=AXIS2_PLACEMENT_3D('',#9711,#7679,#7680);
#6263=AXIS2_PLACEMENT_3D('',#9712,#7681,#7682);
#6264=AXIS2_PLACEMENT_3D('',#9714,#7683,#7684);
#6265=AXIS2_PLACEMENT_3D('',#9715,#7685,#7686);
#6266=AXIS2_PLACEMENT_3D('',#9718,#7688,#7689);
#6267=AXIS2_PLACEMENT_3D('',#9719,#7690,#7691);
#6268=AXIS2_PLACEMENT_3D('',#9720,#7692,#7693);
#6269=AXIS2_PLACEMENT_3D('',#9721,#7694,#7695);
#6270=AXIS2_PLACEMENT_3D('',#9730,#7700,#7701);
#6271=AXIS2_PLACEMENT_3D('',#9736,#7705,#7706);
#6272=AXIS2_PLACEMENT_3D('',#9742,#7710,#7711);
#6273=AXIS2_PLACEMENT_3D('',#9748,#7715,#7716);
#6274=AXIS2_PLACEMENT_3D('',#9754,#7720,#7721);
#6275=AXIS2_PLACEMENT_3D('',#9757,#7724,#7725);
#6276=AXIS2_PLACEMENT_3D('',#9758,#7726,#7727);
#6277=AXIS2_PLACEMENT_3D('',#9759,#7728,#7729);
#6278=AXIS2_PLACEMENT_3D('',#9761,#7730,#7731);
#6279=AXIS2_PLACEMENT_3D('',#9762,#7732,#7733);
#6280=AXIS2_PLACEMENT_3D('',#9764,#7734,#7735);
#6281=AXIS2_PLACEMENT_3D('',#9765,#7736,#7737);
#6282=AXIS2_PLACEMENT_3D('',#9767,#7738,#7739);
#6283=AXIS2_PLACEMENT_3D('',#9769,#7741,#7742);
#6284=AXIS2_PLACEMENT_3D('',#9771,#7743,#7744);
#6285=AXIS2_PLACEMENT_3D('',#9773,#7746,#7747);
#6286=AXIS2_PLACEMENT_3D('',#9775,#7748,#7749);
#6287=AXIS2_PLACEMENT_3D('',#9777,#7751,#7752);
#6288=AXIS2_PLACEMENT_3D('',#9779,#7753,#7754);
#6289=AXIS2_PLACEMENT_3D('',#9780,#7755,#7756);
#6290=AXIS2_PLACEMENT_3D('',#9782,#7757,#7758);
#6291=AXIS2_PLACEMENT_3D('',#9784,#7760,#7761);
#6292=AXIS2_PLACEMENT_3D('',#9786,#7763,#7764);
#6293=AXIS2_PLACEMENT_3D('',#9787,#7765,#7766);
#6294=AXIS2_PLACEMENT_3D('',#9789,#7767,#7768);
#6295=AXIS2_PLACEMENT_3D('',#9792,#7770,#7771);
#6296=AXIS2_PLACEMENT_3D('',#9793,#7772,#7773);
#6297=AXIS2_PLACEMENT_3D('',#9796,#7775,#7776);
#6298=AXIS2_PLACEMENT_3D('',#9797,#7777,#7778);
#6299=AXIS2_PLACEMENT_3D('',#9799,#7779,#7780);
#6300=AXIS2_PLACEMENT_3D('',#9800,#7781,#7782);
#6301=AXIS2_PLACEMENT_3D('',#9803,#7784,#7785);
#6302=AXIS2_PLACEMENT_3D('',#9804,#7786,#7787);
#6303=AXIS2_PLACEMENT_3D('',#9805,#7788,#7789);
#6304=AXIS2_PLACEMENT_3D('',#9806,#7790,#7791);
#6305=AXIS2_PLACEMENT_3D('',#9808,#7792,#7793);
#6306=AXIS2_PLACEMENT_3D('',#9809,#7794,#7795);
#6307=AXIS2_PLACEMENT_3D('',#9811,#7796,#7797);
#6308=AXIS2_PLACEMENT_3D('',#9813,#7799,#7800);
#6309=AXIS2_PLACEMENT_3D('',#9815,#7801,#7802);
#6310=AXIS2_PLACEMENT_3D('',#9817,#7804,#7805);
#6311=AXIS2_PLACEMENT_3D('',#9819,#7806,#7807);
#6312=AXIS2_PLACEMENT_3D('',#9821,#7809,#7810);
#6313=AXIS2_PLACEMENT_3D('',#9823,#7811,#7812);
#6314=AXIS2_PLACEMENT_3D('',#9824,#7813,#7814);
#6315=AXIS2_PLACEMENT_3D('',#9826,#7815,#7816);
#6316=AXIS2_PLACEMENT_3D('',#9828,#7818,#7819);
#6317=AXIS2_PLACEMENT_3D('',#9830,#7820,#7821);
#6318=AXIS2_PLACEMENT_3D('',#9832,#7823,#7824);
#6319=AXIS2_PLACEMENT_3D('',#9834,#7825,#7826);
#6320=AXIS2_PLACEMENT_3D('',#9836,#7828,#7829);
#6321=AXIS2_PLACEMENT_3D('',#9837,#7830,#7831);
#6322=AXIS2_PLACEMENT_3D('',#9846,#7836,#7837);
#6323=AXIS2_PLACEMENT_3D('',#9852,#7841,#7842);
#6324=AXIS2_PLACEMENT_3D('',#9858,#7846,#7847);
#6325=AXIS2_PLACEMENT_3D('',#9864,#7851,#7852);
#6326=AXIS2_PLACEMENT_3D('',#9870,#7856,#7857);
#6327=AXIS2_PLACEMENT_3D('',#9873,#7860,#7861);
#6328=AXIS2_PLACEMENT_3D('',#9874,#7862,#7863);
#6329=AXIS2_PLACEMENT_3D('',#9875,#7864,#7865);
#6330=AXIS2_PLACEMENT_3D('',#9876,#7866,#7867);
#6331=AXIS2_PLACEMENT_3D('',#9877,#7868,#7869);
#6332=AXIS2_PLACEMENT_3D('',#9878,#7870,#7871);
#6333=AXIS2_PLACEMENT_3D('',#9879,#7872,#7873);
#6334=AXIS2_PLACEMENT_3D('',#9880,#7874,#7875);
#6335=AXIS2_PLACEMENT_3D('',#9881,#7876,#7877);
#6336=AXIS2_PLACEMENT_3D('',#9882,#7878,#7879);
#6337=AXIS2_PLACEMENT_3D('',#9883,#7880,#7881);
#6338=AXIS2_PLACEMENT_3D('',#9884,#7882,#7883);
#6339=AXIS2_PLACEMENT_3D('',#9885,#7884,#7885);
#6340=AXIS2_PLACEMENT_3D('',#9886,#7886,#7887);
#6341=AXIS2_PLACEMENT_3D('',#9887,#7888,#7889);
#6342=AXIS2_PLACEMENT_3D('',#9888,#7890,#7891);
#6343=AXIS2_PLACEMENT_3D('',#9889,#7892,#7893);
#6344=AXIS2_PLACEMENT_3D('',#9890,#7894,#7895);
#6345=AXIS2_PLACEMENT_3D('',#9891,#7896,#7897);
#6346=AXIS2_PLACEMENT_3D('',#9892,#7898,#7899);
#6347=AXIS2_PLACEMENT_3D('',#9893,#7900,#7901);
#6348=AXIS2_PLACEMENT_3D('',#9894,#7902,#7903);
#6349=AXIS2_PLACEMENT_3D('',#9895,#7904,#7905);
#6350=AXIS2_PLACEMENT_3D('',#9896,#7906,#7907);
#6351=AXIS2_PLACEMENT_3D('',#9897,#7908,#7909);
#6352=AXIS2_PLACEMENT_3D('',#9898,#7910,#7911);
#6353=AXIS2_PLACEMENT_3D('',#9899,#7912,#7913);
#6354=AXIS2_PLACEMENT_3D('',#9900,#7914,#7915);
#6355=AXIS2_PLACEMENT_3D('',#9901,#7916,#7917);
#6356=AXIS2_PLACEMENT_3D('',#9902,#7918,#7919);
#6357=AXIS2_PLACEMENT_3D('',#9903,#7920,#7921);
#6358=AXIS2_PLACEMENT_3D('',#9904,#7922,#7923);
#6359=AXIS2_PLACEMENT_3D('',#9905,#7924,#7925);
#6360=AXIS2_PLACEMENT_3D('',#9906,#7926,#7927);
#6361=AXIS2_PLACEMENT_3D('',#9907,#7928,#7929);
#6362=AXIS2_PLACEMENT_3D('',#9908,#7930,#7931);
#6363=AXIS2_PLACEMENT_3D('',#9909,#7932,#7933);
#6364=AXIS2_PLACEMENT_3D('',#9910,#7934,#7935);
#6365=AXIS2_PLACEMENT_3D('',#9911,#7936,#7937);
#6366=AXIS2_PLACEMENT_3D('',#9912,#7938,#7939);
#6367=AXIS2_PLACEMENT_3D('',#9913,#7940,#7941);
#6368=AXIS2_PLACEMENT_3D('',#9914,#7942,#7943);
#6369=AXIS2_PLACEMENT_3D('',#9915,#7944,#7945);
#6370=AXIS2_PLACEMENT_3D('',#9916,#7946,#7947);
#6371=AXIS2_PLACEMENT_3D('',#9917,#7948,#7949);
#6372=AXIS2_PLACEMENT_3D('',#9918,#7950,#7951);
#6373=AXIS2_PLACEMENT_3D('',#9919,#7952,#7953);
#6374=AXIS2_PLACEMENT_3D('',#9920,#7954,#7955);
#6375=AXIS2_PLACEMENT_3D('',#9921,#7956,#7957);
#6376=AXIS2_PLACEMENT_3D('',#9922,#7958,#7959);
#6377=AXIS2_PLACEMENT_3D('',#9923,#7960,#7961);
#6378=AXIS2_PLACEMENT_3D('',#9924,#7962,#7963);
#6379=AXIS2_PLACEMENT_3D('',#9925,#7964,#7965);
#6380=AXIS2_PLACEMENT_3D('',#9926,#7966,#7967);
#6381=AXIS2_PLACEMENT_3D('',#9927,#7968,#7969);
#6382=AXIS2_PLACEMENT_3D('',#9928,#7970,#7971);
#6383=AXIS2_PLACEMENT_3D('',#9929,#7972,#7973);
#6384=AXIS2_PLACEMENT_3D('',#9930,#7974,#7975);
#6385=AXIS2_PLACEMENT_3D('',#9931,#7976,#7977);
#6386=AXIS2_PLACEMENT_3D('',#9932,#7978,#7979);
#6387=AXIS2_PLACEMENT_3D('',#9933,#7980,#7981);
#6388=AXIS2_PLACEMENT_3D('',#9934,#7982,#7983);
#6389=AXIS2_PLACEMENT_3D('',#9935,#7984,#7985);
#6390=AXIS2_PLACEMENT_3D('',#9936,#7986,#7987);
#6391=AXIS2_PLACEMENT_3D('',#9937,#7988,#7989);
#6392=AXIS2_PLACEMENT_3D('',#9938,#7990,#7991);
#6393=AXIS2_PLACEMENT_3D('',#9939,#7992,#7993);
#6394=AXIS2_PLACEMENT_3D('',#9940,#7994,#7995);
#6395=AXIS2_PLACEMENT_3D('',#9941,#7996,#7997);
#6396=AXIS2_PLACEMENT_3D('',#9942,#7998,#7999);
#6397=AXIS2_PLACEMENT_3D('',#9943,#8000,#8001);
#6398=AXIS2_PLACEMENT_3D('',#9944,#8002,#8003);
#6399=AXIS2_PLACEMENT_3D('',#9945,#8004,#8005);
#6400=AXIS2_PLACEMENT_3D('',#9946,#8006,#8007);
#6401=AXIS2_PLACEMENT_3D('',#9947,#8008,#8009);
#6402=AXIS2_PLACEMENT_3D('',#9948,#8010,#8011);
#6403=AXIS2_PLACEMENT_3D('',#9949,#8012,#8013);
#6404=AXIS2_PLACEMENT_3D('',#9950,#8014,#8015);
#6405=AXIS2_PLACEMENT_3D('',#9951,#8016,#8017);
#6406=AXIS2_PLACEMENT_3D('',#9952,#8018,#8019);
#6407=AXIS2_PLACEMENT_3D('',#9953,#8020,#8021);
#6408=AXIS2_PLACEMENT_3D('',#9954,#8022,#8023);
#6409=AXIS2_PLACEMENT_3D('',#9955,#8024,#8025);
#6410=AXIS2_PLACEMENT_3D('',#9956,#8026,#8027);
#6411=AXIS2_PLACEMENT_3D('',#9957,#8028,#8029);
#6412=AXIS2_PLACEMENT_3D('',#9958,#8030,#8031);
#6413=AXIS2_PLACEMENT_3D('',#9959,#8032,#8033);
#6414=AXIS2_PLACEMENT_3D('',#9960,#8034,#8035);
#6415=AXIS2_PLACEMENT_3D('',#9961,#8036,#8037);
#6416=AXIS2_PLACEMENT_3D('',#9962,#8038,#8039);
#6417=AXIS2_PLACEMENT_3D('',#9963,#8040,#8041);
#6418=AXIS2_PLACEMENT_3D('',#9964,#8042,#8043);
#6419=AXIS2_PLACEMENT_3D('',#9965,#8044,#8045);
#6420=AXIS2_PLACEMENT_3D('',#9966,#8046,#8047);
#6421=AXIS2_PLACEMENT_3D('',#9967,#8048,#8049);
#6422=AXIS2_PLACEMENT_3D('',#9968,#8050,#8051);
#6423=AXIS2_PLACEMENT_3D('',#9969,#8052,#8053);
#6424=AXIS2_PLACEMENT_3D('',#9970,#8054,#8055);
#6425=AXIS2_PLACEMENT_3D('',#9971,#8056,#8057);
#6426=DIRECTION('axis',(0.,0.,1.));
#6427=DIRECTION('refdir',(1.,0.,0.));
#6428=DIRECTION('axis',(0.,0.,1.));
#6429=DIRECTION('refdir',(1.,0.,0.));
#6430=DIRECTION('center_axis',(0.,0.,1.));
#6431=DIRECTION('ref_axis',(1.,0.,0.));
#6432=DIRECTION('center_axis',(0.,0.,-1.));
#6433=DIRECTION('ref_axis',(1.,0.,0.));
#6434=DIRECTION('',(0.,0.,-1.));
#6435=DIRECTION('center_axis',(0.,0.,-1.));
#6436=DIRECTION('ref_axis',(1.,0.,0.));
#6437=DIRECTION('center_axis',(0.,0.,1.));
#6438=DIRECTION('ref_axis',(1.,0.,0.));
#6439=DIRECTION('center_axis',(0.,0.,1.));
#6440=DIRECTION('ref_axis',(1.,0.,0.));
#6441=DIRECTION('',(0.,0.,-1.));
#6442=DIRECTION('center_axis',(0.,0.,1.));
#6443=DIRECTION('ref_axis',(1.,0.,0.));
#6444=DIRECTION('center_axis',(0.,0.,1.));
#6445=DIRECTION('ref_axis',(1.,0.,0.));
#6446=DIRECTION('center_axis',(0.,0.,1.));
#6447=DIRECTION('ref_axis',(1.,0.,0.));
#6448=DIRECTION('axis',(0.,0.,1.));
#6449=DIRECTION('refdir',(1.,0.,0.));
#6450=DIRECTION('center_axis',(0.,0.,1.));
#6451=DIRECTION('ref_axis',(1.,0.,0.));
#6452=DIRECTION('center_axis',(0.,0.,-1.));
#6453=DIRECTION('ref_axis',(1.,0.,0.));
#6454=DIRECTION('',(0.,0.,-1.));
#6455=DIRECTION('center_axis',(0.,0.,-1.));
#6456=DIRECTION('ref_axis',(1.,0.,0.));
#6457=DIRECTION('center_axis',(0.,0.,1.));
#6458=DIRECTION('ref_axis',(1.,0.,0.));
#6459=DIRECTION('center_axis',(0.,0.,1.));
#6460=DIRECTION('ref_axis',(1.,0.,0.));
#6461=DIRECTION('',(0.,0.,-1.));
#6462=DIRECTION('center_axis',(0.,0.,1.));
#6463=DIRECTION('ref_axis',(1.,0.,0.));
#6464=DIRECTION('center_axis',(0.,0.,1.));
#6465=DIRECTION('ref_axis',(1.,0.,0.));
#6466=DIRECTION('center_axis',(0.,0.,1.));
#6467=DIRECTION('ref_axis',(1.,0.,0.));
#6468=DIRECTION('axis',(0.,0.,1.));
#6469=DIRECTION('refdir',(1.,0.,0.));
#6470=DIRECTION('center_axis',(0.,0.,1.));
#6471=DIRECTION('ref_axis',(1.,0.,0.));
#6472=DIRECTION('center_axis',(0.,0.,-1.));
#6473=DIRECTION('ref_axis',(1.,0.,0.));
#6474=DIRECTION('',(0.,0.,-1.));
#6475=DIRECTION('center_axis',(0.,0.,-1.));
#6476=DIRECTION('ref_axis',(1.,0.,0.));
#6477=DIRECTION('center_axis',(0.,0.,1.));
#6478=DIRECTION('ref_axis',(1.,0.,0.));
#6479=DIRECTION('center_axis',(0.,0.,1.));
#6480=DIRECTION('ref_axis',(1.,0.,0.));
#6481=DIRECTION('',(0.,0.,-1.));
#6482=DIRECTION('center_axis',(0.,0.,1.));
#6483=DIRECTION('ref_axis',(1.,0.,0.));
#6484=DIRECTION('center_axis',(0.,0.,1.));
#6485=DIRECTION('ref_axis',(1.,0.,0.));
#6486=DIRECTION('center_axis',(0.,0.,1.));
#6487=DIRECTION('ref_axis',(1.,0.,0.));
#6488=DIRECTION('axis',(0.,0.,1.));
#6489=DIRECTION('refdir',(1.,0.,0.));
#6490=DIRECTION('center_axis',(0.,0.,1.));
#6491=DIRECTION('ref_axis',(1.,0.,0.));
#6492=DIRECTION('center_axis',(0.,0.,-1.));
#6493=DIRECTION('ref_axis',(1.,0.,0.));
#6494=DIRECTION('',(0.,0.,-1.));
#6495=DIRECTION('center_axis',(0.,0.,-1.));
#6496=DIRECTION('ref_axis',(1.,0.,0.));
#6497=DIRECTION('center_axis',(0.,0.,1.));
#6498=DIRECTION('ref_axis',(1.,0.,0.));
#6499=DIRECTION('center_axis',(0.,0.,1.));
#6500=DIRECTION('ref_axis',(1.,0.,0.));
#6501=DIRECTION('',(0.,0.,-1.));
#6502=DIRECTION('center_axis',(0.,0.,1.));
#6503=DIRECTION('ref_axis',(1.,0.,0.));
#6504=DIRECTION('center_axis',(0.,0.,1.));
#6505=DIRECTION('ref_axis',(1.,0.,0.));
#6506=DIRECTION('center_axis',(0.,0.,1.));
#6507=DIRECTION('ref_axis',(1.,0.,0.));
#6508=DIRECTION('axis',(0.,0.,1.));
#6509=DIRECTION('refdir',(1.,0.,0.));
#6510=DIRECTION('center_axis',(0.,0.,1.));
#6511=DIRECTION('ref_axis',(1.,0.,0.));
#6512=DIRECTION('center_axis',(0.,0.,-1.));
#6513=DIRECTION('ref_axis',(1.,0.,0.));
#6514=DIRECTION('',(0.,0.,-1.));
#6515=DIRECTION('center_axis',(0.,0.,-1.));
#6516=DIRECTION('ref_axis',(1.,0.,0.));
#6517=DIRECTION('center_axis',(0.,0.,1.));
#6518=DIRECTION('ref_axis',(1.,0.,0.));
#6519=DIRECTION('center_axis',(0.,0.,1.));
#6520=DIRECTION('ref_axis',(1.,0.,0.));
#6521=DIRECTION('',(0.,0.,-1.));
#6522=DIRECTION('center_axis',(0.,0.,1.));
#6523=DIRECTION('ref_axis',(1.,0.,0.));
#6524=DIRECTION('center_axis',(0.,0.,1.));
#6525=DIRECTION('ref_axis',(1.,0.,0.));
#6526=DIRECTION('center_axis',(0.,0.,1.));
#6527=DIRECTION('ref_axis',(1.,0.,0.));
#6528=DIRECTION('axis',(0.,0.,1.));
#6529=DIRECTION('refdir',(1.,0.,0.));
#6530=DIRECTION('center_axis',(0.,0.,1.));
#6531=DIRECTION('ref_axis',(1.,0.,0.));
#6532=DIRECTION('center_axis',(0.,0.,-1.));
#6533=DIRECTION('ref_axis',(1.,0.,0.));
#6534=DIRECTION('',(0.,0.,-1.));
#6535=DIRECTION('center_axis',(0.,0.,-1.));
#6536=DIRECTION('ref_axis',(1.,0.,0.));
#6537=DIRECTION('center_axis',(0.,0.,1.));
#6538=DIRECTION('ref_axis',(1.,0.,0.));
#6539=DIRECTION('center_axis',(0.,0.,1.));
#6540=DIRECTION('ref_axis',(1.,0.,0.));
#6541=DIRECTION('',(0.,0.,-1.));
#6542=DIRECTION('center_axis',(0.,0.,1.));
#6543=DIRECTION('ref_axis',(1.,0.,0.));
#6544=DIRECTION('center_axis',(0.,0.,1.));
#6545=DIRECTION('ref_axis',(1.,0.,0.));
#6546=DIRECTION('center_axis',(0.,0.,1.));
#6547=DIRECTION('ref_axis',(1.,0.,0.));
#6548=DIRECTION('axis',(0.,0.,1.));
#6549=DIRECTION('refdir',(1.,0.,0.));
#6550=DIRECTION('center_axis',(0.,0.,1.));
#6551=DIRECTION('ref_axis',(1.,0.,0.));
#6552=DIRECTION('center_axis',(0.,0.,-1.));
#6553=DIRECTION('ref_axis',(1.,0.,0.));
#6554=DIRECTION('',(0.,0.,-1.));
#6555=DIRECTION('center_axis',(0.,0.,-1.));
#6556=DIRECTION('ref_axis',(1.,0.,0.));
#6557=DIRECTION('center_axis',(0.,0.,1.));
#6558=DIRECTION('ref_axis',(1.,0.,0.));
#6559=DIRECTION('center_axis',(0.,0.,1.));
#6560=DIRECTION('ref_axis',(1.,0.,0.));
#6561=DIRECTION('',(0.,0.,-1.));
#6562=DIRECTION('center_axis',(0.,0.,1.));
#6563=DIRECTION('ref_axis',(1.,0.,0.));
#6564=DIRECTION('center_axis',(0.,0.,1.));
#6565=DIRECTION('ref_axis',(1.,0.,0.));
#6566=DIRECTION('center_axis',(0.,0.,1.));
#6567=DIRECTION('ref_axis',(1.,0.,0.));
#6568=DIRECTION('axis',(0.,0.,1.));
#6569=DIRECTION('refdir',(1.,0.,0.));
#6570=DIRECTION('center_axis',(0.,0.,1.));
#6571=DIRECTION('ref_axis',(1.,0.,0.));
#6572=DIRECTION('center_axis',(0.,0.,-1.));
#6573=DIRECTION('ref_axis',(1.,0.,0.));
#6574=DIRECTION('',(0.,0.,-1.));
#6575=DIRECTION('center_axis',(0.,0.,-1.));
#6576=DIRECTION('ref_axis',(1.,0.,0.));
#6577=DIRECTION('center_axis',(0.,0.,1.));
#6578=DIRECTION('ref_axis',(1.,0.,0.));
#6579=DIRECTION('center_axis',(0.,0.,1.));
#6580=DIRECTION('ref_axis',(1.,0.,0.));
#6581=DIRECTION('',(0.,0.,-1.));
#6582=DIRECTION('center_axis',(0.,0.,1.));
#6583=DIRECTION('ref_axis',(1.,0.,0.));
#6584=DIRECTION('center_axis',(0.,0.,1.));
#6585=DIRECTION('ref_axis',(1.,0.,0.));
#6586=DIRECTION('center_axis',(0.,0.,1.));
#6587=DIRECTION('ref_axis',(1.,0.,0.));
#6588=DIRECTION('axis',(0.,0.,1.));
#6589=DIRECTION('refdir',(1.,0.,0.));
#6590=DIRECTION('center_axis',(0.,0.,1.));
#6591=DIRECTION('ref_axis',(1.,0.,0.));
#6592=DIRECTION('center_axis',(0.,0.,1.));
#6593=DIRECTION('ref_axis',(1.,0.,0.));
#6594=DIRECTION('',(0.,0.,1.));
#6595=DIRECTION('center_axis',(0.,0.,-1.));
#6596=DIRECTION('ref_axis',(1.,0.,0.));
#6597=DIRECTION('center_axis',(0.,0.,1.));
#6598=DIRECTION('ref_axis',(1.,0.,0.));
#6599=DIRECTION('center_axis',(0.,0.,1.));
#6600=DIRECTION('ref_axis',(1.,0.,0.));
#6601=DIRECTION('center_axis',(0.,0.,1.));
#6602=DIRECTION('ref_axis',(1.,0.,0.));
#6603=DIRECTION('center_axis',(0.,0.,1.));
#6604=DIRECTION('ref_axis',(1.,0.,0.));
#6605=DIRECTION('',(0.,0.,1.));
#6606=DIRECTION('center_axis',(0.,0.,-1.));
#6607=DIRECTION('ref_axis',(1.,0.,0.));
#6608=DIRECTION('center_axis',(0.,0.,1.));
#6609=DIRECTION('ref_axis',(1.,0.,0.));
#6610=DIRECTION('center_axis',(0.,0.,1.));
#6611=DIRECTION('ref_axis',(1.,0.,0.));
#6612=DIRECTION('center_axis',(0.,0.,1.));
#6613=DIRECTION('ref_axis',(1.,0.,0.));
#6614=DIRECTION('center_axis',(0.,0.,1.));
#6615=DIRECTION('ref_axis',(1.,0.,0.));
#6616=DIRECTION('',(0.,0.,1.));
#6617=DIRECTION('center_axis',(0.,0.,-1.));
#6618=DIRECTION('ref_axis',(1.,0.,0.));
#6619=DIRECTION('center_axis',(0.,0.,1.));
#6620=DIRECTION('ref_axis',(1.,0.,0.));
#6621=DIRECTION('center_axis',(0.,0.,1.));
#6622=DIRECTION('ref_axis',(1.,0.,0.));
#6623=DIRECTION('center_axis',(0.,0.,1.));
#6624=DIRECTION('ref_axis',(1.,0.,0.));
#6625=DIRECTION('center_axis',(0.,0.,1.));
#6626=DIRECTION('ref_axis',(1.,0.,0.));
#6627=DIRECTION('',(0.,0.,1.));
#6628=DIRECTION('center_axis',(0.,0.,-1.));
#6629=DIRECTION('ref_axis',(1.,0.,0.));
#6630=DIRECTION('center_axis',(0.,0.,1.));
#6631=DIRECTION('ref_axis',(1.,0.,0.));
#6632=DIRECTION('center_axis',(0.,0.,1.));
#6633=DIRECTION('ref_axis',(1.,0.,0.));
#6634=DIRECTION('center_axis',(0.,0.,1.));
#6635=DIRECTION('ref_axis',(1.,0.,0.));
#6636=DIRECTION('center_axis',(0.,0.,1.));
#6637=DIRECTION('ref_axis',(1.,0.,0.));
#6638=DIRECTION('',(0.,0.,1.));
#6639=DIRECTION('center_axis',(0.,0.,1.));
#6640=DIRECTION('ref_axis',(1.,0.,0.));
#6641=DIRECTION('center_axis',(0.,0.,1.));
#6642=DIRECTION('ref_axis',(1.,0.,0.));
#6643=DIRECTION('',(0.,0.,1.));
#6644=DIRECTION('center_axis',(0.,0.,1.));
#6645=DIRECTION('ref_axis',(1.,0.,0.));
#6646=DIRECTION('center_axis',(0.,0.,1.));
#6647=DIRECTION('ref_axis',(1.,0.,0.));
#6648=DIRECTION('',(0.,0.,1.));
#6649=DIRECTION('center_axis',(0.,0.,1.));
#6650=DIRECTION('ref_axis',(1.,0.,0.));
#6651=DIRECTION('center_axis',(0.,0.,1.));
#6652=DIRECTION('ref_axis',(1.,0.,0.));
#6653=DIRECTION('',(0.,0.,1.));
#6654=DIRECTION('center_axis',(0.,1.,0.));
#6655=DIRECTION('ref_axis',(-1.,0.,0.));
#6656=DIRECTION('',(-1.,0.,0.));
#6657=DIRECTION('',(0.,0.,1.));
#6658=DIRECTION('',(-1.,0.,0.));
#6659=DIRECTION('',(0.,0.,1.));
#6660=DIRECTION('center_axis',(1.,0.,0.));
#6661=DIRECTION('ref_axis',(0.,1.,0.));
#6662=DIRECTION('',(0.,1.,0.));
#6663=DIRECTION('',(0.,1.,0.));
#6664=DIRECTION('',(0.,0.,1.));
#6665=DIRECTION('center_axis',(0.,-1.,0.));
#6666=DIRECTION('ref_axis',(1.,0.,0.));
#6667=DIRECTION('',(1.,0.,0.));
#6668=DIRECTION('',(1.,0.,0.));
#6669=DIRECTION('',(0.,0.,1.));
#6670=DIRECTION('center_axis',(-1.,0.,0.));
#6671=DIRECTION('ref_axis',(0.,-1.,0.));
#6672=DIRECTION('',(0.,-1.,0.));
#6673=DIRECTION('',(0.,-1.,0.));
#6674=DIRECTION('center_axis',(0.,0.,1.));
#6675=DIRECTION('ref_axis',(1.,0.,0.));
#6676=DIRECTION('center_axis',(0.,0.,1.));
#6677=DIRECTION('ref_axis',(1.,0.,0.));
#6678=DIRECTION('axis',(0.,0.,1.));
#6679=DIRECTION('refdir',(1.,0.,0.));
#6680=DIRECTION('center_axis',(0.,0.,1.));
#6681=DIRECTION('ref_axis',(1.,0.,0.));
#6682=DIRECTION('center_axis',(0.,0.,1.));
#6683=DIRECTION('ref_axis',(1.,0.,0.));
#6684=DIRECTION('',(0.,0.,1.));
#6685=DIRECTION('center_axis',(0.,0.,-1.));
#6686=DIRECTION('ref_axis',(1.,0.,0.));
#6687=DIRECTION('center_axis',(0.,0.,1.));
#6688=DIRECTION('ref_axis',(1.,0.,0.));
#6689=DIRECTION('center_axis',(0.,0.,1.));
#6690=DIRECTION('ref_axis',(1.,0.,0.));
#6691=DIRECTION('',(0.,0.,1.));
#6692=DIRECTION('center_axis',(0.,0.,-1.));
#6693=DIRECTION('ref_axis',(1.,0.,0.));
#6694=DIRECTION('center_axis',(0.,0.,1.));
#6695=DIRECTION('ref_axis',(1.,0.,0.));
#6696=DIRECTION('center_axis',(0.,0.,1.));
#6697=DIRECTION('ref_axis',(1.,0.,0.));
#6698=DIRECTION('',(0.,0.,1.));
#6699=DIRECTION('center_axis',(0.,0.,-1.));
#6700=DIRECTION('ref_axis',(1.,0.,0.));
#6701=DIRECTION('center_axis',(0.,0.,1.));
#6702=DIRECTION('ref_axis',(1.,0.,0.));
#6703=DIRECTION('center_axis',(0.,0.,1.));
#6704=DIRECTION('ref_axis',(1.,0.,0.));
#6705=DIRECTION('',(0.,0.,1.));
#6706=DIRECTION('center_axis',(0.,0.,-1.));
#6707=DIRECTION('ref_axis',(1.,0.,0.));
#6708=DIRECTION('center_axis',(0.,-1.,0.));
#6709=DIRECTION('ref_axis',(1.,0.,0.));
#6710=DIRECTION('',(1.,0.,0.));
#6711=DIRECTION('',(0.,0.,1.));
#6712=DIRECTION('',(-1.,0.,0.));
#6713=DIRECTION('',(0.,0.,1.));
#6714=DIRECTION('center_axis',(-1.,0.,0.));
#6715=DIRECTION('ref_axis',(0.,-1.,0.));
#6716=DIRECTION('',(0.,-1.,0.));
#6717=DIRECTION('',(0.,0.,-1.));
#6718=DIRECTION('',(0.,1.,0.));
#6719=DIRECTION('center_axis',(1.,0.,0.));
#6720=DIRECTION('ref_axis',(0.,1.,0.));
#6721=DIRECTION('',(0.,1.,0.));
#6722=DIRECTION('',(0.,0.,-1.));
#6723=DIRECTION('',(0.,1.,0.));
#6724=DIRECTION('center_axis',(0.,0.,1.));
#6725=DIRECTION('ref_axis',(1.,0.,0.));
#6726=DIRECTION('',(-1.,0.,0.));
#6727=DIRECTION('',(0.,-1.,0.));
#6728=DIRECTION('',(-1.,0.,0.));
#6729=DIRECTION('',(0.,-1.,0.));
#6730=DIRECTION('',(1.,0.,0.));
#6731=DIRECTION('',(0.,-1.,0.));
#6732=DIRECTION('',(1.,0.,0.));
#6733=DIRECTION('',(0.,1.,0.));
#6734=DIRECTION('',(1.,0.,0.));
#6735=DIRECTION('center_axis',(-1.,0.,0.));
#6736=DIRECTION('ref_axis',(0.,-1.,0.));
#6737=DIRECTION('',(0.,-1.,0.));
#6738=DIRECTION('',(0.,0.,1.));
#6739=DIRECTION('',(0.,0.,1.));
#6740=DIRECTION('center_axis',(0.,1.,0.));
#6741=DIRECTION('ref_axis',(-1.,0.,0.));
#6742=DIRECTION('',(-1.,0.,0.));
#6743=DIRECTION('center_axis',(0.,-1.,0.));
#6744=DIRECTION('ref_axis',(1.,0.,0.));
#6745=DIRECTION('',(0.,0.,-1.));
#6746=DIRECTION('',(1.,0.,0.));
#6747=DIRECTION('center_axis',(1.,0.,0.));
#6748=DIRECTION('ref_axis',(0.,1.,0.));
#6749=DIRECTION('',(0.,1.,0.));
#6750=DIRECTION('',(0.,0.,1.));
#6751=DIRECTION('',(0.,0.,1.));
#6752=DIRECTION('center_axis',(0.,-1.,0.));
#6753=DIRECTION('ref_axis',(1.,0.,0.));
#6754=DIRECTION('',(1.,0.,0.));
#6755=DIRECTION('',(0.,0.,-1.));
#6756=DIRECTION('center_axis',(0.,1.,0.));
#6757=DIRECTION('ref_axis',(-1.,0.,0.));
#6758=DIRECTION('',(-1.,0.,0.));
#6759=DIRECTION('center_axis',(1.,0.,0.));
#6760=DIRECTION('ref_axis',(0.,1.,0.));
#6761=DIRECTION('',(0.,0.,1.));
#6762=DIRECTION('',(0.,1.,0.));
#6763=DIRECTION('center_axis',(0.,1.,0.));
#6764=DIRECTION('ref_axis',(-1.,0.,0.));
#6765=DIRECTION('',(0.,0.,1.));
#6766=DIRECTION('',(-1.,0.,0.));
#6767=DIRECTION('center_axis',(-1.,0.,0.));
#6768=DIRECTION('ref_axis',(0.,-1.,0.));
#6769=DIRECTION('',(0.,-1.,0.));
#6770=DIRECTION('center_axis',(0.,0.,1.));
#6771=DIRECTION('ref_axis',(1.,0.,0.));
#6772=DIRECTION('axis',(0.,0.,1.));
#6773=DIRECTION('refdir',(1.,0.,0.));
#6774=DIRECTION('center_axis',(0.,0.,1.));
#6775=DIRECTION('ref_axis',(1.,0.,0.));
#6776=DIRECTION('center_axis',(0.,0.,1.));
#6777=DIRECTION('ref_axis',(1.,0.,0.));
#6778=DIRECTION('',(0.,0.,1.));
#6779=DIRECTION('center_axis',(0.,0.,-1.));
#6780=DIRECTION('ref_axis',(1.,0.,0.));
#6781=DIRECTION('center_axis',(0.,1.,0.));
#6782=DIRECTION('ref_axis',(1.,0.,0.));
#6783=DIRECTION('center_axis',(0.,1.,0.));
#6784=DIRECTION('ref_axis',(1.,0.,0.));
#6785=DIRECTION('',(0.,1.,0.));
#6786=DIRECTION('center_axis',(0.,-1.,0.));
#6787=DIRECTION('ref_axis',(1.,0.,0.));
#6788=DIRECTION('center_axis',(0.,1.,0.));
#6789=DIRECTION('ref_axis',(1.,0.,0.));
#6790=DIRECTION('center_axis',(0.,1.,0.));
#6791=DIRECTION('ref_axis',(1.,0.,0.));
#6792=DIRECTION('',(0.,1.,0.));
#6793=DIRECTION('center_axis',(0.,-1.,0.));
#6794=DIRECTION('ref_axis',(1.,0.,0.));
#6795=DIRECTION('center_axis',(0.,0.,1.));
#6796=DIRECTION('ref_axis',(0.,-1.,0.));
#6797=DIRECTION('',(0.,-1.,0.));
#6798=DIRECTION('',(1.,0.,0.));
#6799=DIRECTION('',(0.,-1.,0.));
#6800=DIRECTION('',(1.,0.,0.));
#6801=DIRECTION('center_axis',(0.,1.,0.));
#6802=DIRECTION('ref_axis',(0.,0.,1.));
#6803=DIRECTION('',(0.,0.,1.));
#6804=DIRECTION('',(0.,0.,1.));
#6805=DIRECTION('',(1.,0.,0.));
#6806=DIRECTION('center_axis',(0.,0.,-1.));
#6807=DIRECTION('ref_axis',(0.,1.,0.));
#6808=DIRECTION('',(0.,1.,0.));
#6809=DIRECTION('',(0.,1.,0.));
#6810=DIRECTION('',(1.,0.,0.));
#6811=DIRECTION('center_axis',(0.,1.,0.));
#6812=DIRECTION('ref_axis',(0.,0.,1.));
#6813=DIRECTION('',(0.,0.,1.));
#6814=DIRECTION('',(0.,0.,1.));
#6815=DIRECTION('',(1.,0.,0.));
#6816=DIRECTION('center_axis',(0.,0.,-1.));
#6817=DIRECTION('ref_axis',(0.,1.,0.));
#6818=DIRECTION('',(0.,1.,0.));
#6819=DIRECTION('',(0.,1.,0.));
#6820=DIRECTION('',(1.,0.,0.));
#6821=DIRECTION('center_axis',(0.,-1.,0.));
#6822=DIRECTION('ref_axis',(0.,0.,-1.));
#6823=DIRECTION('',(0.,0.,-1.));
#6824=DIRECTION('',(0.,0.,-1.));
#6825=DIRECTION('center_axis',(1.,0.,0.));
#6826=DIRECTION('ref_axis',(0.,0.,-1.));
#6827=DIRECTION('center_axis',(1.,0.,0.));
#6828=DIRECTION('ref_axis',(0.,0.,-1.));
#6829=DIRECTION('axis',(0.,0.,1.));
#6830=DIRECTION('refdir',(1.,0.,0.));
#6831=DIRECTION('center_axis',(0.,0.,1.));
#6832=DIRECTION('ref_axis',(1.,0.,0.));
#6833=DIRECTION('center_axis',(0.,0.,1.));
#6834=DIRECTION('ref_axis',(1.,0.,0.));
#6835=DIRECTION('',(0.,0.,1.));
#6836=DIRECTION('center_axis',(0.,0.,-1.));
#6837=DIRECTION('ref_axis',(1.,0.,0.));
#6838=DIRECTION('center_axis',(0.,1.,0.));
#6839=DIRECTION('ref_axis',(1.,0.,0.));
#6840=DIRECTION('center_axis',(0.,1.,0.));
#6841=DIRECTION('ref_axis',(1.,0.,0.));
#6842=DIRECTION('',(0.,1.,0.));
#6843=DIRECTION('center_axis',(0.,-1.,0.));
#6844=DIRECTION('ref_axis',(1.,0.,0.));
#6845=DIRECTION('center_axis',(0.,1.,0.));
#6846=DIRECTION('ref_axis',(1.,0.,0.));
#6847=DIRECTION('center_axis',(0.,1.,0.));
#6848=DIRECTION('ref_axis',(1.,0.,0.));
#6849=DIRECTION('',(0.,1.,0.));
#6850=DIRECTION('center_axis',(0.,-1.,0.));
#6851=DIRECTION('ref_axis',(1.,0.,0.));
#6852=DIRECTION('center_axis',(0.,0.,1.));
#6853=DIRECTION('ref_axis',(0.,-1.,0.));
#6854=DIRECTION('',(0.,-1.,0.));
#6855=DIRECTION('',(1.,0.,0.));
#6856=DIRECTION('',(0.,-1.,0.));
#6857=DIRECTION('',(1.,0.,0.));
#6858=DIRECTION('center_axis',(0.,1.,0.));
#6859=DIRECTION('ref_axis',(0.,0.,1.));
#6860=DIRECTION('',(0.,0.,1.));
#6861=DIRECTION('',(0.,0.,1.));
#6862=DIRECTION('',(1.,0.,0.));
#6863=DIRECTION('center_axis',(0.,0.,-1.));
#6864=DIRECTION('ref_axis',(0.,1.,0.));
#6865=DIRECTION('',(0.,1.,0.));
#6866=DIRECTION('',(0.,1.,0.));
#6867=DIRECTION('',(1.,0.,0.));
#6868=DIRECTION('center_axis',(0.,1.,0.));
#6869=DIRECTION('ref_axis',(0.,0.,1.));
#6870=DIRECTION('',(0.,0.,1.));
#6871=DIRECTION('',(0.,0.,1.));
#6872=DIRECTION('',(1.,0.,0.));
#6873=DIRECTION('center_axis',(0.,0.,-1.));
#6874=DIRECTION('ref_axis',(0.,1.,0.));
#6875=DIRECTION('',(0.,1.,0.));
#6876=DIRECTION('',(0.,1.,0.));
#6877=DIRECTION('',(1.,0.,0.));
#6878=DIRECTION('center_axis',(0.,-1.,0.));
#6879=DIRECTION('ref_axis',(0.,0.,-1.));
#6880=DIRECTION('',(0.,0.,-1.));
#6881=DIRECTION('',(0.,0.,-1.));
#6882=DIRECTION('center_axis',(1.,0.,0.));
#6883=DIRECTION('ref_axis',(0.,0.,-1.));
#6884=DIRECTION('center_axis',(1.,0.,0.));
#6885=DIRECTION('ref_axis',(0.,0.,-1.));
#6886=DIRECTION('axis',(0.,0.,1.));
#6887=DIRECTION('refdir',(1.,0.,0.));
#6888=DIRECTION('center_axis',(0.,0.,1.));
#6889=DIRECTION('ref_axis',(1.,0.,0.));
#6890=DIRECTION('center_axis',(0.,0.,1.));
#6891=DIRECTION('ref_axis',(1.,0.,0.));
#6892=DIRECTION('',(0.,0.,1.));
#6893=DIRECTION('center_axis',(0.,0.,-1.));
#6894=DIRECTION('ref_axis',(1.,0.,0.));
#6895=DIRECTION('center_axis',(0.,0.,1.));
#6896=DIRECTION('ref_axis',(1.,0.,0.));
#6897=DIRECTION('center_axis',(0.,0.,1.));
#6898=DIRECTION('ref_axis',(1.,0.,0.));
#6899=DIRECTION('',(0.,0.,1.));
#6900=DIRECTION('center_axis',(0.,0.,-1.));
#6901=DIRECTION('ref_axis',(1.,0.,0.));
#6902=DIRECTION('center_axis',(0.,1.,0.));
#6903=DIRECTION('ref_axis',(-1.,0.,0.));
#6904=DIRECTION('',(-1.,0.,0.));
#6905=DIRECTION('',(0.,0.,1.));
#6906=DIRECTION('',(-1.,0.,0.));
#6907=DIRECTION('',(0.,0.,1.));
#6908=DIRECTION('center_axis',(1.,0.,0.));
#6909=DIRECTION('ref_axis',(0.,1.,0.));
#6910=DIRECTION('',(0.,1.,0.));
#6911=DIRECTION('',(0.,1.,0.));
#6912=DIRECTION('',(0.,0.,1.));
#6913=DIRECTION('center_axis',(0.,-1.,0.));
#6914=DIRECTION('ref_axis',(1.,0.,0.));
#6915=DIRECTION('',(1.,0.,0.));
#6916=DIRECTION('',(1.,0.,0.));
#6917=DIRECTION('',(0.,0.,1.));
#6918=DIRECTION('center_axis',(-1.,0.,0.));
#6919=DIRECTION('ref_axis',(0.,-1.,0.));
#6920=DIRECTION('',(0.,-1.,0.));
#6921=DIRECTION('',(0.,-1.,0.));
#6922=DIRECTION('center_axis',(0.,0.,1.));
#6923=DIRECTION('ref_axis',(1.,0.,0.));
#6924=DIRECTION('center_axis',(0.,0.,1.));
#6925=DIRECTION('ref_axis',(1.,0.,0.));
#6926=DIRECTION('axis',(0.,0.,1.));
#6927=DIRECTION('refdir',(1.,0.,0.));
#6928=DIRECTION('center_axis',(0.,1.,0.));
#6929=DIRECTION('ref_axis',(1.,0.,0.));
#6930=DIRECTION('center_axis',(0.,1.,0.));
#6931=DIRECTION('ref_axis',(1.,0.,0.));
#6932=DIRECTION('',(0.,1.,0.));
#6933=DIRECTION('',(0.,1.,0.));
#6934=DIRECTION('center_axis',(0.,-1.,2.77555756156289E-16));
#6935=DIRECTION('ref_axis',(1.,0.,0.));
#6936=DIRECTION('center_axis',(0.,1.,0.));
#6937=DIRECTION('ref_axis',(1.,0.,0.));
#6938=DIRECTION('center_axis',(0.,1.,0.));
#6939=DIRECTION('ref_axis',(1.,0.,0.));
#6940=DIRECTION('',(0.,1.,0.));
#6941=DIRECTION('',(0.,1.,0.));
#6942=DIRECTION('center_axis',(0.,-1.,2.77555756156289E-16));
#6943=DIRECTION('ref_axis',(1.,0.,0.));
#6944=DIRECTION('center_axis',(1.,0.,0.));
#6945=DIRECTION('ref_axis',(0.,0.,-1.));
#6946=DIRECTION('',(1.,0.,0.));
#6947=DIRECTION('center_axis',(1.,0.,0.));
#6948=DIRECTION('ref_axis',(0.,0.,-1.));
#6949=DIRECTION('',(1.,0.,0.));
#6950=DIRECTION('center_axis',(0.,0.,1.));
#6951=DIRECTION('ref_axis',(1.,0.,0.));
#6952=DIRECTION('center_axis',(0.,0.,1.));
#6953=DIRECTION('ref_axis',(1.,0.,0.));
#6954=DIRECTION('',(0.,0.,1.));
#6955=DIRECTION('',(0.,0.,1.));
#6956=DIRECTION('center_axis',(0.,0.,-1.));
#6957=DIRECTION('ref_axis',(1.,0.,0.));
#6958=DIRECTION('center_axis',(0.,0.,1.));
#6959=DIRECTION('ref_axis',(1.,0.,0.));
#6960=DIRECTION('center_axis',(0.,0.,1.));
#6961=DIRECTION('ref_axis',(1.,0.,0.));
#6962=DIRECTION('',(0.,0.,1.));
#6963=DIRECTION('',(0.,0.,1.));
#6964=DIRECTION('center_axis',(0.,0.,-1.));
#6965=DIRECTION('ref_axis',(1.,0.,0.));
#6966=DIRECTION('center_axis',(1.,0.,0.));
#6967=DIRECTION('ref_axis',(0.,0.,-1.));
#6968=DIRECTION('',(1.,0.,0.));
#6969=DIRECTION('center_axis',(1.,0.,0.));
#6970=DIRECTION('ref_axis',(0.,0.,-1.));
#6971=DIRECTION('center_axis',(1.,0.,0.));
#6972=DIRECTION('ref_axis',(0.,0.,-1.));
#6973=DIRECTION('',(1.,0.,0.));
#6974=DIRECTION('center_axis',(0.,0.,-1.));
#6975=DIRECTION('ref_axis',(0.,1.,0.));
#6976=DIRECTION('',(0.,1.,0.));
#6977=DIRECTION('',(1.,0.,0.));
#6978=DIRECTION('',(0.,-1.,0.));
#6979=DIRECTION('',(1.,0.,0.));
#6980=DIRECTION('center_axis',(0.,1.,-8.88178419700125E-16));
#6981=DIRECTION('ref_axis',(0.,8.88178419700125E-16,1.));
#6982=DIRECTION('',(0.,8.88178419700125E-16,1.));
#6983=DIRECTION('',(1.,0.,0.));
#6984=DIRECTION('',(0.,-8.88178419700125E-16,-1.));
#6985=DIRECTION('center_axis',(0.,-7.40148683083439E-16,-1.));
#6986=DIRECTION('ref_axis',(0.,1.,-7.40148683083439E-16));
#6987=DIRECTION('',(0.,1.,-7.40148683083439E-16));
#6988=DIRECTION('',(1.,0.,0.));
#6989=DIRECTION('',(0.,-1.,7.40148683083439E-16));
#6990=DIRECTION('center_axis',(0.,-0.707106781186547,-0.707106781186548));
#6991=DIRECTION('ref_axis',(0.,0.707106781186548,-0.707106781186547));
#6992=DIRECTION('',(0.,0.707106781186548,-0.707106781186547));
#6993=DIRECTION('',(1.,0.,0.));
#6994=DIRECTION('',(0.,-0.707106781186548,0.707106781186547));
#6995=DIRECTION('center_axis',(0.,-1.,2.77555756156289E-16));
#6996=DIRECTION('ref_axis',(0.,-2.77555756156289E-16,-1.));
#6997=DIRECTION('',(0.,-2.77555756156289E-16,-1.));
#6998=DIRECTION('',(1.,0.,0.));
#6999=DIRECTION('',(0.,2.77555756156289E-16,1.));
#7000=DIRECTION('center_axis',(0.,-0.707106781186547,0.707106781186548));
#7001=DIRECTION('ref_axis',(0.,-0.707106781186548,-0.707106781186547));
#7002=DIRECTION('',(0.,-0.707106781186548,-0.707106781186547));
#7003=DIRECTION('',(1.,0.,0.));
#7004=DIRECTION('',(0.,0.707106781186548,0.707106781186547));
#7005=DIRECTION('center_axis',(0.,7.40148683083438E-16,1.));
#7006=DIRECTION('ref_axis',(0.,-1.,7.40148683083438E-16));
#7007=DIRECTION('',(0.,-1.,7.40148683083438E-16));
#7008=DIRECTION('',(1.,0.,0.));
#7009=DIRECTION('',(0.,1.,-7.40148683083438E-16));
#7010=DIRECTION('center_axis',(0.,1.,-4.44089209850063E-16));
#7011=DIRECTION('ref_axis',(0.,4.44089209850063E-16,1.));
#7012=DIRECTION('',(0.,4.44089209850063E-16,1.));
#7013=DIRECTION('',(1.,0.,0.));
#7014=DIRECTION('',(0.,-4.44089209850063E-16,-1.));
#7015=DIRECTION('center_axis',(0.,2.41352831440251E-16,1.));
#7016=DIRECTION('ref_axis',(0.,-1.,2.41352831440251E-16));
#7017=DIRECTION('',(0.,-1.,2.41352831440251E-16));
#7018=DIRECTION('',(-1.,0.,0.));
#7019=DIRECTION('',(0.,1.,-2.41352831440251E-16));
#7020=DIRECTION('center_axis',(0.,-1.,2.41352831440251E-16));
#7021=DIRECTION('ref_axis',(0.,-2.41352831440251E-16,-1.));
#7022=DIRECTION('',(0.,-2.41352831440251E-16,-1.));
#7023=DIRECTION('',(1.,0.,0.));
#7024=DIRECTION('',(0.,2.41352831440251E-16,1.));
#7025=DIRECTION('',(1.,0.,0.));
#7026=DIRECTION('center_axis',(0.,0.,-1.));
#7027=DIRECTION('ref_axis',(0.,1.,0.));
#7028=DIRECTION('',(0.,1.,0.));
#7029=DIRECTION('',(1.,0.,0.));
#7030=DIRECTION('',(0.,-1.,0.));
#7031=DIRECTION('center_axis',(0.,-1.,0.));
#7032=DIRECTION('ref_axis',(0.,0.,-1.));
#7033=DIRECTION('',(0.,0.,-1.));
#7034=DIRECTION('',(1.,0.,0.));
#7035=DIRECTION('',(0.,0.,1.));
#7036=DIRECTION('center_axis',(0.,-0.707106781186547,0.707106781186548));
#7037=DIRECTION('ref_axis',(0.,-0.707106781186548,-0.707106781186547));
#7038=DIRECTION('',(0.,-0.707106781186548,-0.707106781186547));
#7039=DIRECTION('',(1.,0.,0.));
#7040=DIRECTION('',(0.,0.707106781186548,0.707106781186547));
#7041=DIRECTION('center_axis',(0.,0.,1.));
#7042=DIRECTION('ref_axis',(0.,-1.,0.));
#7043=DIRECTION('',(0.,-1.,0.));
#7044=DIRECTION('',(1.,0.,0.));
#7045=DIRECTION('',(0.,1.,0.));
#7046=DIRECTION('center_axis',(0.,0.707106781186548,0.707106781186547));
#7047=DIRECTION('ref_axis',(0.,-0.707106781186547,0.707106781186548));
#7048=DIRECTION('',(0.,-0.707106781186547,0.707106781186548));
#7049=DIRECTION('',(1.,0.,0.));
#7050=DIRECTION('',(0.,0.707106781186547,-0.707106781186548));
#7051=DIRECTION('center_axis',(0.,1.,0.));
#7052=DIRECTION('ref_axis',(0.,0.,1.));
#7053=DIRECTION('',(0.,0.,1.));
#7054=DIRECTION('',(1.,0.,0.));
#7055=DIRECTION('',(0.,0.,-1.));
#7056=DIRECTION('center_axis',(0.,0.,-1.));
#7057=DIRECTION('ref_axis',(0.,1.,0.));
#7058=DIRECTION('',(0.,1.,0.));
#7059=DIRECTION('',(1.,0.,0.));
#7060=DIRECTION('',(0.,-1.,0.));
#7061=DIRECTION('center_axis',(0.,1.,-2.41352831440251E-16));
#7062=DIRECTION('ref_axis',(0.,2.41352831440251E-16,1.));
#7063=DIRECTION('',(0.,2.41352831440251E-16,1.));
#7064=DIRECTION('',(-1.,0.,0.));
#7065=DIRECTION('',(0.,-2.41352831440251E-16,-1.));
#7066=DIRECTION('center_axis',(0.,0.,1.));
#7067=DIRECTION('ref_axis',(0.,-1.,0.));
#7068=DIRECTION('',(0.,-1.,0.));
#7069=DIRECTION('',(1.,0.,0.));
#7070=DIRECTION('',(0.,1.,0.));
#7071=DIRECTION('',(1.,0.,0.));
#7072=DIRECTION('center_axis',(0.,-1.,0.));
#7073=DIRECTION('ref_axis',(0.,0.,-1.));
#7074=DIRECTION('',(0.,0.,-1.));
#7075=DIRECTION('',(1.,0.,0.));
#7076=DIRECTION('',(0.,0.,1.));
#7077=DIRECTION('center_axis',(0.,0.,1.));
#7078=DIRECTION('ref_axis',(0.,-1.,0.));
#7079=DIRECTION('',(0.,-1.,0.));
#7080=DIRECTION('',(1.,0.,0.));
#7081=DIRECTION('',(0.,1.,0.));
#7082=DIRECTION('center_axis',(0.,0.707106781186548,0.707106781186548));
#7083=DIRECTION('ref_axis',(0.,-0.707106781186548,0.707106781186548));
#7084=DIRECTION('',(0.,-0.707106781186548,0.707106781186548));
#7085=DIRECTION('',(1.,0.,0.));
#7086=DIRECTION('',(0.,0.707106781186548,-0.707106781186548));
#7087=DIRECTION('center_axis',(0.,1.,0.));
#7088=DIRECTION('ref_axis',(0.,0.,1.));
#7089=DIRECTION('',(0.,0.,1.));
#7090=DIRECTION('',(1.,0.,0.));
#7091=DIRECTION('',(0.,0.,-1.));
#7092=DIRECTION('center_axis',(0.,0.707106781186548,-0.707106781186547));
#7093=DIRECTION('ref_axis',(0.,0.707106781186547,0.707106781186548));
#7094=DIRECTION('',(0.,0.707106781186547,0.707106781186548));
#7095=DIRECTION('',(1.,0.,0.));
#7096=DIRECTION('',(0.,-0.707106781186547,-0.707106781186548));
#7097=DIRECTION('center_axis',(0.,-7.40148683083438E-16,-1.));
#7098=DIRECTION('ref_axis',(0.,1.,-7.40148683083438E-16));
#7099=DIRECTION('',(0.,1.,-7.40148683083438E-16));
#7100=DIRECTION('',(1.,0.,0.));
#7101=DIRECTION('',(0.,-1.,7.40148683083438E-16));
#7102=DIRECTION('center_axis',(0.,-1.,0.));
#7103=DIRECTION('ref_axis',(0.,0.,-1.));
#7104=DIRECTION('',(0.,0.,-1.));
#7105=DIRECTION('',(1.,0.,0.));
#7106=DIRECTION('',(0.,0.,1.));
#7107=DIRECTION('center_axis',(0.,0.,-1.));
#7108=DIRECTION('ref_axis',(0.,1.,0.));
#7109=DIRECTION('',(0.,1.,0.));
#7110=DIRECTION('',(-1.,0.,0.));
#7111=DIRECTION('',(0.,-1.,0.));
#7112=DIRECTION('center_axis',(0.,1.,0.));
#7113=DIRECTION('ref_axis',(0.,0.,1.));
#7114=DIRECTION('',(0.,0.,1.));
#7115=DIRECTION('',(1.,0.,0.));
#7116=DIRECTION('',(0.,0.,-1.));
#7117=DIRECTION('',(1.,0.,0.));
#7118=DIRECTION('center_axis',(0.,0.,1.));
#7119=DIRECTION('ref_axis',(0.,-1.,0.));
#7120=DIRECTION('',(0.,-1.,0.));
#7121=DIRECTION('',(1.,0.,0.));
#7122=DIRECTION('',(0.,1.,0.));
#7123=DIRECTION('center_axis',(0.,1.,0.));
#7124=DIRECTION('ref_axis',(0.,0.,1.));
#7125=DIRECTION('',(0.,0.,1.));
#7126=DIRECTION('',(1.,0.,0.));
#7127=DIRECTION('',(0.,0.,-1.));
#7128=DIRECTION('center_axis',(0.,0.707106781186547,-0.707106781186548));
#7129=DIRECTION('ref_axis',(0.,0.707106781186548,0.707106781186547));
#7130=DIRECTION('',(0.,0.707106781186548,0.707106781186547));
#7131=DIRECTION('',(1.,0.,0.));
#7132=DIRECTION('',(0.,-0.707106781186548,-0.707106781186547));
#7133=DIRECTION('center_axis',(0.,0.,-1.));
#7134=DIRECTION('ref_axis',(0.,1.,0.));
#7135=DIRECTION('',(0.,1.,0.));
#7136=DIRECTION('',(1.,0.,0.));
#7137=DIRECTION('',(0.,-1.,0.));
#7138=DIRECTION('center_axis',(0.,-0.707106781186547,-0.707106781186548));
#7139=DIRECTION('ref_axis',(0.,0.707106781186548,-0.707106781186547));
#7140=DIRECTION('',(0.,0.707106781186548,-0.707106781186547));
#7141=DIRECTION('',(1.,0.,0.));
#7142=DIRECTION('',(0.,-0.707106781186548,0.707106781186547));
#7143=DIRECTION('center_axis',(0.,-1.,0.));
#7144=DIRECTION('ref_axis',(0.,0.,-1.));
#7145=DIRECTION('',(0.,0.,-1.));
#7146=DIRECTION('',(1.,0.,0.));
#7147=DIRECTION('',(0.,0.,1.));
#7148=DIRECTION('center_axis',(0.,0.,1.));
#7149=DIRECTION('ref_axis',(0.,-1.,0.));
#7150=DIRECTION('',(0.,-1.,0.));
#7151=DIRECTION('',(1.,0.,0.));
#7152=DIRECTION('',(0.,1.,0.));
#7153=DIRECTION('center_axis',(0.,-1.,0.));
#7154=DIRECTION('ref_axis',(0.,0.,-1.));
#7155=DIRECTION('',(0.,0.,-1.));
#7156=DIRECTION('',(-1.,0.,0.));
#7157=DIRECTION('',(0.,0.,1.));
#7158=DIRECTION('center_axis',(1.,0.,0.));
#7159=DIRECTION('ref_axis',(0.,0.,-1.));
#7160=DIRECTION('',(1.,0.,0.));
#7161=DIRECTION('center_axis',(-1.,0.,0.));
#7162=DIRECTION('ref_axis',(0.,0.,-1.));
#7163=DIRECTION('center_axis',(0.,1.,0.));
#7164=DIRECTION('ref_axis',(0.,0.,1.));
#7165=DIRECTION('',(0.,0.,1.));
#7166=DIRECTION('',(1.,0.,0.));
#7167=DIRECTION('',(0.,0.,1.));
#7168=DIRECTION('center_axis',(0.,1.,0.));
#7169=DIRECTION('ref_axis',(0.,0.,1.));
#7170=DIRECTION('',(0.,0.,1.));
#7171=DIRECTION('',(1.,0.,0.));
#7172=DIRECTION('',(0.,0.,1.));
#7173=DIRECTION('center_axis',(0.,0.,-1.));
#7174=DIRECTION('ref_axis',(0.,1.,0.));
#7175=DIRECTION('',(0.,1.,0.));
#7176=DIRECTION('',(0.,1.,0.));
#7177=DIRECTION('center_axis',(0.,0.,-1.));
#7178=DIRECTION('ref_axis',(0.,1.,0.));
#7179=DIRECTION('',(0.,1.,0.));
#7180=DIRECTION('',(1.,0.,0.));
#7181=DIRECTION('',(0.,1.,0.));
#7182=DIRECTION('center_axis',(0.,-1.,0.));
#7183=DIRECTION('ref_axis',(0.,0.,-1.));
#7184=DIRECTION('',(0.,0.,-1.));
#7185=DIRECTION('',(0.,0.,-1.));
#7186=DIRECTION('center_axis',(0.,-1.,0.));
#7187=DIRECTION('ref_axis',(0.,0.,-1.));
#7188=DIRECTION('',(0.,0.,-1.));
#7189=DIRECTION('',(1.,0.,0.));
#7190=DIRECTION('',(0.,0.,-1.));
#7191=DIRECTION('center_axis',(0.,0.,1.));
#7192=DIRECTION('ref_axis',(0.,-1.,0.));
#7193=DIRECTION('',(0.,-1.,0.));
#7194=DIRECTION('',(0.,-1.,0.));
#7195=DIRECTION('center_axis',(0.,0.,1.));
#7196=DIRECTION('ref_axis',(0.,-1.,0.));
#7197=DIRECTION('',(0.,-1.,0.));
#7198=DIRECTION('',(0.,-1.,0.));
#7199=DIRECTION('center_axis',(1.,0.,0.));
#7200=DIRECTION('ref_axis',(0.,0.,-1.));
#7201=DIRECTION('center_axis',(1.,0.,0.));
#7202=DIRECTION('ref_axis',(0.,0.,-1.));
#7203=DIRECTION('axis',(0.,0.,1.));
#7204=DIRECTION('refdir',(1.,0.,0.));
#7205=DIRECTION('center_axis',(1.,0.,0.));
#7206=DIRECTION('ref_axis',(0.,0.,-1.));
#7207=DIRECTION('',(0.,0.,1.));
#7208=DIRECTION('',(0.,-1.,0.));
#7209=DIRECTION('',(0.,0.,1.));
#7210=DIRECTION('',(0.,0.707106781186548,0.707106781186547));
#7211=DIRECTION('',(0.,1.,0.));
#7212=DIRECTION('',(0.,0.707106781186548,-0.707106781186547));
#7213=DIRECTION('',(0.,0.,-1.));
#7214=DIRECTION('',(0.,-1.,0.));
#7215=DIRECTION('',(0.,0.,-1.));
#7216=DIRECTION('',(0.,1.,0.));
#7217=DIRECTION('',(0.,0.,1.));
#7218=DIRECTION('',(0.,-1.,0.));
#7219=DIRECTION('',(0.,0.,-1.));
#7220=DIRECTION('',(0.,-1.,0.));
#7221=DIRECTION('',(0.,-0.707106781186548,0.707106781186548));
#7222=DIRECTION('',(0.,0.,1.));
#7223=DIRECTION('',(0.,0.707106781186547,0.707106781186548));
#7224=DIRECTION('',(0.,1.,-7.40148683083438E-16));
#7225=DIRECTION('',(0.,0.,-1.));
#7226=DIRECTION('',(0.,1.,0.));
#7227=DIRECTION('',(0.,0.,1.));
#7228=DIRECTION('',(0.,-1.,0.));
#7229=DIRECTION('',(0.,-2.41352831440251E-16,-1.));
#7230=DIRECTION('',(0.,1.,0.));
#7231=DIRECTION('',(0.,0.,-1.));
#7232=DIRECTION('',(0.,-0.707106781186548,-0.707106781186547));
#7233=DIRECTION('',(0.,-1.,0.));
#7234=DIRECTION('',(0.,-0.707106781186547,0.707106781186548));
#7235=DIRECTION('',(0.,0.,1.));
#7236=DIRECTION('',(0.,1.,0.));
#7237=DIRECTION('',(0.,2.41352831440251E-16,1.));
#7238=DIRECTION('',(0.,-1.,0.));
#7239=DIRECTION('',(0.,0.,-1.));
#7240=DIRECTION('',(0.,1.,0.));
#7241=DIRECTION('',(0.,8.88178419700125E-16,1.));
#7242=DIRECTION('',(0.,1.,-7.40148683083439E-16));
#7243=DIRECTION('',(0.,0.707106781186548,-0.707106781186547));
#7244=DIRECTION('',(0.,-2.77555756156289E-16,-1.));
#7245=DIRECTION('',(0.,-0.707106781186548,-0.707106781186547));
#7246=DIRECTION('',(0.,-1.,7.40148683083438E-16));
#7247=DIRECTION('',(0.,4.44089209850063E-16,1.));
#7248=DIRECTION('',(0.,-1.,2.41352831440251E-16));
#7249=DIRECTION('',(0.,0.,-1.));
#7250=DIRECTION('',(0.,1.,0.));
#7251=DIRECTION('center_axis',(1.,0.,0.));
#7252=DIRECTION('ref_axis',(0.,0.,-1.));
#7253=DIRECTION('center_axis',(0.,-1.,2.41352831440251E-16));
#7254=DIRECTION('ref_axis',(0.,-2.41352831440251E-16,-1.));
#7255=DIRECTION('',(1.,0.,0.));
#7256=DIRECTION('',(0.,-2.41352831440251E-16,-1.));
#7257=DIRECTION('',(1.,0.,0.));
#7258=DIRECTION('center_axis',(0.,0.,-1.));
#7259=DIRECTION('ref_axis',(0.,1.,0.));
#7260=DIRECTION('',(1.,0.,0.));
#7261=DIRECTION('',(0.,1.,0.));
#7262=DIRECTION('center_axis',(0.,-1.,0.));
#7263=DIRECTION('ref_axis',(0.,0.,-1.));
#7264=DIRECTION('',(-1.,0.,0.));
#7265=DIRECTION('',(0.,0.,-1.));
#7266=DIRECTION('center_axis',(0.,0.,-1.));
#7267=DIRECTION('ref_axis',(0.,1.,0.));
#7268=DIRECTION('',(1.,0.,0.));
#7269=DIRECTION('',(0.,1.,0.));
#7270=DIRECTION('center_axis',(0.,-1.,0.));
#7271=DIRECTION('ref_axis',(0.,0.,-1.));
#7272=DIRECTION('',(1.,0.,0.));
#7273=DIRECTION('',(0.,0.,-1.));
#7274=DIRECTION('center_axis',(0.,-7.40148683083438E-16,-1.));
#7275=DIRECTION('ref_axis',(0.,1.,-7.40148683083438E-16));
#7276=DIRECTION('',(1.,0.,0.));
#7277=DIRECTION('',(0.,1.,-7.40148683083438E-16));
#7278=DIRECTION('center_axis',(0.,0.707106781186548,-0.707106781186547));
#7279=DIRECTION('ref_axis',(0.,0.707106781186547,0.707106781186548));
#7280=DIRECTION('',(1.,0.,0.));
#7281=DIRECTION('',(0.,0.707106781186547,0.707106781186548));
#7282=DIRECTION('center_axis',(0.,1.,0.));
#7283=DIRECTION('ref_axis',(0.,0.,1.));
#7284=DIRECTION('',(1.,0.,0.));
#7285=DIRECTION('',(0.,0.,1.));
#7286=DIRECTION('center_axis',(0.,0.707106781186548,0.707106781186548));
#7287=DIRECTION('ref_axis',(0.,-0.707106781186548,0.707106781186548));
#7288=DIRECTION('',(1.,0.,0.));
#7289=DIRECTION('',(0.,-0.707106781186548,0.707106781186548));
#7290=DIRECTION('center_axis',(0.,0.,1.));
#7291=DIRECTION('ref_axis',(0.,-1.,0.));
#7292=DIRECTION('',(1.,0.,0.));
#7293=DIRECTION('',(0.,-1.,0.));
#7294=DIRECTION('center_axis',(0.,-1.,0.));
#7295=DIRECTION('ref_axis',(0.,0.,-1.));
#7296=DIRECTION('',(1.,0.,0.));
#7297=DIRECTION('',(0.,0.,-1.));
#7298=DIRECTION('center_axis',(0.,0.,1.));
#7299=DIRECTION('ref_axis',(0.,-1.,0.));
#7300=DIRECTION('',(1.,0.,0.));
#7301=DIRECTION('',(0.,-1.,0.));
#7302=DIRECTION('center_axis',(0.,-1.,0.));
#7303=DIRECTION('ref_axis',(0.,0.,-1.));
#7304=DIRECTION('',(1.,0.,0.));
#7305=DIRECTION('',(0.,0.,-1.));
#7306=DIRECTION('center_axis',(0.,0.,1.));
#7307=DIRECTION('ref_axis',(0.,-1.,0.));
#7308=DIRECTION('',(-1.,0.,0.));
#7309=DIRECTION('',(0.,-1.,0.));
#7310=DIRECTION('center_axis',(0.,-1.,0.));
#7311=DIRECTION('ref_axis',(0.,0.,-1.));
#7312=DIRECTION('',(1.,0.,0.));
#7313=DIRECTION('',(0.,0.,-1.));
#7314=DIRECTION('center_axis',(0.,0.,1.));
#7315=DIRECTION('ref_axis',(0.,-1.,0.));
#7316=DIRECTION('',(1.,0.,0.));
#7317=DIRECTION('',(0.,-1.,0.));
#7318=DIRECTION('center_axis',(0.,-1.,0.));
#7319=DIRECTION('ref_axis',(0.,0.,-1.));
#7320=DIRECTION('',(1.,0.,0.));
#7321=DIRECTION('',(0.,0.,-1.));
#7322=DIRECTION('center_axis',(0.,-0.707106781186547,-0.707106781186548));
#7323=DIRECTION('ref_axis',(0.,0.707106781186548,-0.707106781186547));
#7324=DIRECTION('',(1.,0.,0.));
#7325=DIRECTION('',(0.,0.707106781186548,-0.707106781186547));
#7326=DIRECTION('center_axis',(0.,0.,-1.));
#7327=DIRECTION('ref_axis',(0.,1.,0.));
#7328=DIRECTION('',(1.,0.,0.));
#7329=DIRECTION('',(0.,1.,0.));
#7330=DIRECTION('center_axis',(0.,0.707106781186547,-0.707106781186548));
#7331=DIRECTION('ref_axis',(0.,0.707106781186548,0.707106781186547));
#7332=DIRECTION('',(1.,0.,0.));
#7333=DIRECTION('',(0.,0.707106781186548,0.707106781186547));
#7334=DIRECTION('center_axis',(0.,1.,0.));
#7335=DIRECTION('ref_axis',(0.,0.,1.));
#7336=DIRECTION('',(1.,0.,0.));
#7337=DIRECTION('',(0.,0.,1.));
#7338=DIRECTION('center_axis',(0.,0.,1.));
#7339=DIRECTION('ref_axis',(0.,-1.,0.));
#7340=DIRECTION('',(1.,0.,0.));
#7341=DIRECTION('',(0.,-1.,0.));
#7342=DIRECTION('center_axis',(0.,0.,-1.));
#7343=DIRECTION('ref_axis',(0.,1.,0.));
#7344=DIRECTION('',(1.,0.,0.));
#7345=DIRECTION('',(0.,1.,0.));
#7346=DIRECTION('',(1.,0.,0.));
#7347=DIRECTION('center_axis',(0.,1.,-8.88178419700125E-16));
#7348=DIRECTION('ref_axis',(0.,8.88178419700125E-16,1.));
#7349=DIRECTION('',(0.,8.88178419700125E-16,1.));
#7350=DIRECTION('',(1.,0.,0.));
#7351=DIRECTION('center_axis',(0.,-7.40148683083439E-16,-1.));
#7352=DIRECTION('ref_axis',(0.,1.,-7.40148683083439E-16));
#7353=DIRECTION('',(0.,1.,-7.40148683083439E-16));
#7354=DIRECTION('',(1.,0.,0.));
#7355=DIRECTION('center_axis',(0.,-0.707106781186547,-0.707106781186548));
#7356=DIRECTION('ref_axis',(0.,0.707106781186548,-0.707106781186547));
#7357=DIRECTION('',(0.,0.707106781186548,-0.707106781186547));
#7358=DIRECTION('',(1.,0.,0.));
#7359=DIRECTION('center_axis',(0.,-1.,2.77555756156289E-16));
#7360=DIRECTION('ref_axis',(0.,-2.77555756156289E-16,-1.));
#7361=DIRECTION('',(0.,-2.77555756156289E-16,-1.));
#7362=DIRECTION('',(1.,0.,0.));
#7363=DIRECTION('center_axis',(0.,-0.707106781186547,0.707106781186548));
#7364=DIRECTION('ref_axis',(0.,-0.707106781186548,-0.707106781186547));
#7365=DIRECTION('',(0.,-0.707106781186548,-0.707106781186547));
#7366=DIRECTION('',(1.,0.,0.));
#7367=DIRECTION('center_axis',(0.,7.40148683083438E-16,1.));
#7368=DIRECTION('ref_axis',(0.,-1.,7.40148683083438E-16));
#7369=DIRECTION('',(0.,-1.,7.40148683083438E-16));
#7370=DIRECTION('',(1.,0.,0.));
#7371=DIRECTION('center_axis',(0.,1.,-4.44089209850063E-16));
#7372=DIRECTION('ref_axis',(0.,4.44089209850063E-16,1.));
#7373=DIRECTION('',(0.,4.44089209850063E-16,1.));
#7374=DIRECTION('',(1.,0.,0.));
#7375=DIRECTION('center_axis',(0.,2.41352831440251E-16,1.));
#7376=DIRECTION('ref_axis',(0.,-1.,2.41352831440251E-16));
#7377=DIRECTION('',(0.,-1.,2.41352831440251E-16));
#7378=DIRECTION('',(-1.,0.,0.));
#7379=DIRECTION('center_axis',(0.,0.,-1.));
#7380=DIRECTION('ref_axis',(0.,1.,0.));
#7381=DIRECTION('',(0.,1.,0.));
#7382=DIRECTION('',(1.,0.,0.));
#7383=DIRECTION('center_axis',(0.,-1.,0.));
#7384=DIRECTION('ref_axis',(0.,0.,-1.));
#7385=DIRECTION('',(0.,0.,-1.));
#7386=DIRECTION('',(1.,0.,0.));
#7387=DIRECTION('center_axis',(0.,-0.707106781186547,0.707106781186548));
#7388=DIRECTION('ref_axis',(0.,-0.707106781186548,-0.707106781186547));
#7389=DIRECTION('',(0.,-0.707106781186548,-0.707106781186547));
#7390=DIRECTION('',(1.,0.,0.));
#7391=DIRECTION('center_axis',(0.,0.,1.));
#7392=DIRECTION('ref_axis',(0.,-1.,0.));
#7393=DIRECTION('',(0.,-1.,0.));
#7394=DIRECTION('',(1.,0.,0.));
#7395=DIRECTION('center_axis',(0.,0.707106781186548,0.707106781186547));
#7396=DIRECTION('ref_axis',(0.,-0.707106781186547,0.707106781186548));
#7397=DIRECTION('',(0.,-0.707106781186547,0.707106781186548));
#7398=DIRECTION('',(1.,0.,0.));
#7399=DIRECTION('center_axis',(0.,1.,0.));
#7400=DIRECTION('ref_axis',(0.,0.,1.));
#7401=DIRECTION('',(0.,0.,1.));
#7402=DIRECTION('',(1.,0.,0.));
#7403=DIRECTION('center_axis',(0.,0.,-1.));
#7404=DIRECTION('ref_axis',(0.,1.,0.));
#7405=DIRECTION('',(0.,1.,0.));
#7406=DIRECTION('',(1.,0.,0.));
#7407=DIRECTION('center_axis',(0.,1.,-2.41352831440251E-16));
#7408=DIRECTION('ref_axis',(0.,2.41352831440251E-16,1.));
#7409=DIRECTION('',(0.,2.41352831440251E-16,1.));
#7410=DIRECTION('',(-1.,0.,0.));
#7411=DIRECTION('center_axis',(0.,1.,0.));
#7412=DIRECTION('ref_axis',(0.,0.,1.));
#7413=DIRECTION('',(1.,0.,0.));
#7414=DIRECTION('',(0.,0.,1.));
#7415=DIRECTION('center_axis',(1.,0.,0.));
#7416=DIRECTION('ref_axis',(0.,0.,-1.));
#7417=DIRECTION('center_axis',(1.,0.,0.));
#7418=DIRECTION('ref_axis',(0.,0.,-1.));
#7419=DIRECTION('',(1.,0.,0.));
#7420=DIRECTION('center_axis',(0.,1.,0.));
#7421=DIRECTION('ref_axis',(0.,0.,1.));
#7422=DIRECTION('',(0.,0.,1.));
#7423=DIRECTION('',(1.,0.,0.));
#7424=DIRECTION('center_axis',(0.,1.,0.));
#7425=DIRECTION('ref_axis',(0.,0.,1.));
#7426=DIRECTION('',(1.,0.,0.));
#7427=DIRECTION('',(0.,0.,1.));
#7428=DIRECTION('center_axis',(0.,0.,-1.));
#7429=DIRECTION('ref_axis',(0.,1.,0.));
#7430=DIRECTION('',(0.,1.,0.));
#7431=DIRECTION('center_axis',(0.,0.,1.));
#7432=DIRECTION('ref_axis',(0.,-1.,0.));
#7433=DIRECTION('',(0.,-1.,0.));
#7434=DIRECTION('center_axis',(1.,0.,0.));
#7435=DIRECTION('ref_axis',(0.,0.,-1.));
#7436=DIRECTION('axis',(0.,0.,1.));
#7437=DIRECTION('refdir',(1.,0.,0.));
#7438=DIRECTION('center_axis',(0.866025403784439,0.,-0.5));
#7439=DIRECTION('ref_axis',(0.5,0.,0.866025403784439));
#7440=DIRECTION('',(-0.5,0.,-0.866025403784439));
#7441=DIRECTION('',(0.,-1.,0.));
#7442=DIRECTION('',(0.5,0.,0.866025403784439));
#7443=DIRECTION('',(0.,-1.,0.));
#7444=DIRECTION('center_axis',(1.20185167898973E-16,0.,-1.));
#7445=DIRECTION('ref_axis',(1.,0.,1.20185167898973E-16));
#7446=DIRECTION('',(-1.,0.,-1.20185167898973E-16));
#7447=DIRECTION('',(0.,-1.,0.));
#7448=DIRECTION('',(1.,0.,1.20185167898973E-16));
#7449=DIRECTION('center_axis',(-0.866025403784439,0.,-0.5));
#7450=DIRECTION('ref_axis',(0.5,0.,-0.866025403784439));
#7451=DIRECTION('',(-0.5,0.,0.866025403784439));
#7452=DIRECTION('',(0.,-1.,0.));
#7453=DIRECTION('',(0.5,0.,-0.866025403784439));
#7454=DIRECTION('center_axis',(-0.866025403784439,0.,0.5));
#7455=DIRECTION('ref_axis',(-0.5,0.,-0.866025403784439));
#7456=DIRECTION('',(0.5,0.,0.866025403784439));
#7457=DIRECTION('',(0.,-1.,0.));
#7458=DIRECTION('',(-0.5,0.,-0.866025403784439));
#7459=DIRECTION('center_axis',(-2.40370335797945E-16,0.,1.));
#7460=DIRECTION('ref_axis',(-1.,0.,-2.40370335797945E-16));
#7461=DIRECTION('',(1.,0.,2.40370335797945E-16));
#7462=DIRECTION('',(0.,-1.,0.));
#7463=DIRECTION('',(-1.,0.,-2.40370335797945E-16));
#7464=DIRECTION('center_axis',(0.866025403784439,0.,0.5));
#7465=DIRECTION('ref_axis',(-0.5,0.,0.866025403784439));
#7466=DIRECTION('',(0.5,0.,-0.866025403784439));
#7467=DIRECTION('',(-0.5,0.,0.866025403784439));
#7468=DIRECTION('center_axis',(0.,1.,0.));
#7469=DIRECTION('ref_axis',(1.,0.,0.));
#7470=DIRECTION('center_axis',(0.,-1.,0.));
#7471=DIRECTION('ref_axis',(0.,0.,-1.));
#7472=DIRECTION('center_axis',(0.,1.,0.));
#7473=DIRECTION('ref_axis',(1.,0.,0.));
#7474=DIRECTION('center_axis',(0.,1.,0.));
#7475=DIRECTION('ref_axis',(1.,0.,0.));
#7476=DIRECTION('center_axis',(0.,1.,0.));
#7477=DIRECTION('ref_axis',(1.,0.,0.));
#7478=DIRECTION('center_axis',(0.,1.,0.));
#7479=DIRECTION('ref_axis',(1.,0.,0.));
#7480=DIRECTION('',(0.,-1.,0.));
#7481=DIRECTION('center_axis',(0.,1.,0.));
#7482=DIRECTION('ref_axis',(1.,0.,0.));
#7483=DIRECTION('center_axis',(0.,1.,0.));
#7484=DIRECTION('ref_axis',(1.,0.,0.));
#7485=DIRECTION('center_axis',(0.,1.,0.));
#7486=DIRECTION('ref_axis',(0.,0.,1.));
#7487=DIRECTION('center_axis',(0.,-1.,0.));
#7488=DIRECTION('ref_axis',(1.,0.,0.));
#7489=DIRECTION('center_axis',(0.,-1.,0.));
#7490=DIRECTION('ref_axis',(1.,0.,0.));
#7491=DIRECTION('center_axis',(0.,-1.,0.));
#7492=DIRECTION('ref_axis',(1.,0.,0.));
#7493=DIRECTION('',(0.707106781186548,0.707106781186547,8.65956056235493E-17));
#7494=DIRECTION('center_axis',(0.,-1.,0.));
#7495=DIRECTION('ref_axis',(1.,0.,0.));
#7496=DIRECTION('center_axis',(0.,-1.,0.));
#7497=DIRECTION('ref_axis',(1.,0.,0.));
#7498=DIRECTION('',(0.,1.,0.));
#7499=DIRECTION('center_axis',(0.,1.,0.));
#7500=DIRECTION('ref_axis',(1.,0.,0.));
#7501=DIRECTION('center_axis',(0.,-1.,0.));
#7502=DIRECTION('ref_axis',(1.,0.,0.));
#7503=DIRECTION('',(-0.707106781186547,0.707106781186548,-8.65956056235493E-17));
#7504=DIRECTION('center_axis',(0.,-1.,0.));
#7505=DIRECTION('ref_axis',(0.,0.,-1.));
#7506=DIRECTION('center_axis',(0.,-1.,0.));
#7507=DIRECTION('ref_axis',(1.,0.,0.));
#7508=DIRECTION('center_axis',(0.,1.,0.));
#7509=DIRECTION('ref_axis',(1.,0.,0.));
#7510=DIRECTION('center_axis',(0.,1.,0.));
#7511=DIRECTION('ref_axis',(1.,0.,0.));
#7512=DIRECTION('',(-0.447213595499958,0.894427190999916,-5.47678698264203E-17));
#7513=DIRECTION('center_axis',(0.,-1.,0.));
#7514=DIRECTION('ref_axis',(1.,0.,0.));
#7515=DIRECTION('',(0.,1.,0.));
#7516=DIRECTION('axis',(0.,0.,1.));
#7517=DIRECTION('refdir',(1.,0.,0.));
#7518=DIRECTION('center_axis',(0.,1.,0.));
#7519=DIRECTION('ref_axis',(0.,0.,1.));
#7520=DIRECTION('center_axis',(0.,-1.,0.));
#7521=DIRECTION('ref_axis',(1.,0.,0.));
#7522=DIRECTION('center_axis',(0.,-1.,0.));
#7523=DIRECTION('ref_axis',(1.,0.,0.));
#7524=DIRECTION('center_axis',(0.,-1.,0.));
#7525=DIRECTION('ref_axis',(1.,0.,0.));
#7526=DIRECTION('',(0.707106781186548,0.707106781186547,8.65956056235493E-17));
#7527=DIRECTION('center_axis',(0.,-1.,0.));
#7528=DIRECTION('ref_axis',(1.,0.,0.));
#7529=DIRECTION('center_axis',(0.,-1.,0.));
#7530=DIRECTION('ref_axis',(1.,0.,0.));
#7531=DIRECTION('',(0.,1.,0.));
#7532=DIRECTION('center_axis',(0.,1.,0.));
#7533=DIRECTION('ref_axis',(1.,0.,0.));
#7534=DIRECTION('center_axis',(0.,-1.,0.));
#7535=DIRECTION('ref_axis',(1.,0.,0.));
#7536=DIRECTION('',(-0.707106781186547,0.707106781186548,-8.65956056235493E-17));
#7537=DIRECTION('center_axis',(0.,-1.,0.));
#7538=DIRECTION('ref_axis',(0.,0.,-1.));
#7539=DIRECTION('center_axis',(0.,-1.,0.));
#7540=DIRECTION('ref_axis',(1.,0.,0.));
#7541=DIRECTION('center_axis',(0.,1.,0.));
#7542=DIRECTION('ref_axis',(1.,0.,0.));
#7543=DIRECTION('center_axis',(0.,1.,0.));
#7544=DIRECTION('ref_axis',(1.,0.,0.));
#7545=DIRECTION('',(-0.447213595499958,0.894427190999916,-5.47678698264203E-17));
#7546=DIRECTION('center_axis',(0.,-1.,0.));
#7547=DIRECTION('ref_axis',(1.,0.,0.));
#7548=DIRECTION('center_axis',(0.,1.,0.));
#7549=DIRECTION('ref_axis',(1.,0.,0.));
#7550=DIRECTION('',(0.,1.,0.));
#7551=DIRECTION('center_axis',(0.,1.,0.));
#7552=DIRECTION('ref_axis',(1.,0.,0.));
#7553=DIRECTION('center_axis',(0.,-1.,0.));
#7554=DIRECTION('ref_axis',(1.,0.,0.));
#7555=DIRECTION('',(-0.707106781186547,0.707106781186548,-8.65956056235493E-17));
#7556=DIRECTION('center_axis',(0.,-1.,0.));
#7557=DIRECTION('ref_axis',(0.,0.,-1.));
#7558=DIRECTION('center_axis',(0.866025403784439,0.,-0.5));
#7559=DIRECTION('ref_axis',(0.5,0.,0.866025403784439));
#7560=DIRECTION('',(-0.5,0.,-0.866025403784439));
#7561=DIRECTION('',(0.,-1.,0.));
#7562=DIRECTION('',(0.5,0.,0.866025403784439));
#7563=DIRECTION('',(0.,-1.,0.));
#7564=DIRECTION('center_axis',(1.20185167898973E-16,0.,-1.));
#7565=DIRECTION('ref_axis',(1.,0.,1.20185167898973E-16));
#7566=DIRECTION('',(-1.,0.,-1.20185167898973E-16));
#7567=DIRECTION('',(0.,-1.,0.));
#7568=DIRECTION('',(1.,0.,1.20185167898973E-16));
#7569=DIRECTION('center_axis',(-0.866025403784439,0.,-0.5));
#7570=DIRECTION('ref_axis',(0.5,0.,-0.866025403784439));
#7571=DIRECTION('',(-0.5,0.,0.866025403784439));
#7572=DIRECTION('',(0.,-1.,0.));
#7573=DIRECTION('',(0.5,0.,-0.866025403784439));
#7574=DIRECTION('center_axis',(-0.866025403784439,0.,0.5));
#7575=DIRECTION('ref_axis',(-0.5,0.,-0.866025403784439));
#7576=DIRECTION('',(0.5,0.,0.866025403784439));
#7577=DIRECTION('',(0.,-1.,0.));
#7578=DIRECTION('',(-0.5,0.,-0.866025403784439));
#7579=DIRECTION('center_axis',(-2.40370335797945E-16,0.,1.));
#7580=DIRECTION('ref_axis',(-1.,0.,-2.40370335797945E-16));
#7581=DIRECTION('',(1.,0.,2.40370335797945E-16));
#7582=DIRECTION('',(0.,-1.,0.));
#7583=DIRECTION('',(-1.,0.,-2.40370335797945E-16));
#7584=DIRECTION('center_axis',(0.866025403784439,0.,0.5));
#7585=DIRECTION('ref_axis',(-0.5,0.,0.866025403784439));
#7586=DIRECTION('',(0.5,0.,-0.866025403784439));
#7587=DIRECTION('',(-0.5,0.,0.866025403784439));
#7588=DIRECTION('center_axis',(0.,1.,0.));
#7589=DIRECTION('ref_axis',(1.,0.,0.));
#7590=DIRECTION('center_axis',(0.,-1.,0.));
#7591=DIRECTION('ref_axis',(0.,0.,-1.));
#7592=DIRECTION('axis',(0.,0.,1.));
#7593=DIRECTION('refdir',(1.,0.,0.));
#7594=DIRECTION('center_axis',(0.,0.,1.));
#7595=DIRECTION('ref_axis',(1.,0.,0.));
#7596=DIRECTION('',(1.,0.,0.));
#7597=DIRECTION('',(0.,-1.,0.));
#7598=DIRECTION('',(-1.,0.,0.));
#7599=DIRECTION('',(0.,1.,0.));
#7600=DIRECTION('center_axis',(0.,1.,0.));
#7601=DIRECTION('ref_axis',(-1.,0.,0.));
#7602=DIRECTION('',(0.,0.,1.));
#7603=DIRECTION('',(-1.,0.,0.));
#7604=DIRECTION('',(0.,0.,1.));
#7605=DIRECTION('center_axis',(0.,0.,1.));
#7606=DIRECTION('ref_axis',(1.,0.,0.));
#7607=DIRECTION('',(0.,-1.,0.));
#7608=DIRECTION('',(1.,0.,0.));
#7609=DIRECTION('',(0.,1.,0.));
#7610=DIRECTION('center_axis',(0.,0.,-1.));
#7611=DIRECTION('ref_axis',(1.,0.,0.));
#7612=DIRECTION('center_axis',(-1.,0.,0.));
#7613=DIRECTION('ref_axis',(0.,-1.,0.));
#7614=DIRECTION('',(0.,0.,1.));
#7615=DIRECTION('',(0.,0.707106781186548,0.707106781186548));
#7616=DIRECTION('',(0.,-1.,0.));
#7617=DIRECTION('',(0.,0.707106781186548,-0.707106781186548));
#7618=DIRECTION('',(0.,0.,1.));
#7619=DIRECTION('',(0.,-1.,0.));
#7620=DIRECTION('',(0.,0.,1.));
#7621=DIRECTION('center_axis',(0.,-1.,0.));
#7622=DIRECTION('ref_axis',(1.,0.,0.));
#7623=DIRECTION('',(1.,0.,0.));
#7624=DIRECTION('',(0.,0.,1.));
#7625=DIRECTION('center_axis',(0.,0.,1.));
#7626=DIRECTION('ref_axis',(1.,0.,0.));
#7627=DIRECTION('',(-1.,0.,0.));
#7628=DIRECTION('',(0.,1.,0.));
#7629=DIRECTION('center_axis',(1.,0.,0.));
#7630=DIRECTION('ref_axis',(0.,1.,0.));
#7631=DIRECTION('',(0.,0.,1.));
#7632=DIRECTION('',(0.,-0.707106781186548,0.707106781186548));
#7633=DIRECTION('',(0.,1.,0.));
#7634=DIRECTION('',(0.,-0.707106781186548,-0.707106781186548));
#7635=DIRECTION('',(0.,0.,1.));
#7636=DIRECTION('center_axis',(0.,-1.,0.));
#7637=DIRECTION('ref_axis',(1.,0.,0.));
#7638=DIRECTION('',(-1.,0.,0.));
#7639=DIRECTION('center_axis',(0.,-0.707106781186548,-0.707106781186548));
#7640=DIRECTION('ref_axis',(-1.,0.,0.));
#7641=DIRECTION('',(1.,0.,0.));
#7642=DIRECTION('center_axis',(0.,0.707106781186548,0.707106781186548));
#7643=DIRECTION('ref_axis',(0.,0.707106781186547,-0.707106781186547));
#7644=DIRECTION('',(1.,0.,0.));
#7645=DIRECTION('center_axis',(0.,0.,1.));
#7646=DIRECTION('ref_axis',(1.,0.,0.));
#7647=DIRECTION('center_axis',(0.,0.,-1.));
#7648=DIRECTION('ref_axis',(1.,0.,0.));
#7649=DIRECTION('',(0.,0.,1.));
#7650=DIRECTION('center_axis',(0.,0.,-1.));
#7651=DIRECTION('ref_axis',(1.,0.,0.));
#7652=DIRECTION('center_axis',(0.,-0.707106781186548,0.707106781186548));
#7653=DIRECTION('ref_axis',(0.,0.707106781186547,0.707106781186547));
#7654=DIRECTION('center_axis',(0.,0.,-1.));
#7655=DIRECTION('ref_axis',(1.,0.,0.));
#7656=DIRECTION('center_axis',(0.,0.,1.));
#7657=DIRECTION('ref_axis',(1.,0.,0.));
#7658=DIRECTION('',(-1.,0.,0.));
#7659=DIRECTION('center_axis',(0.,0.,1.));
#7660=DIRECTION('ref_axis',(1.,0.,0.));
#7661=DIRECTION('',(-1.,0.,0.));
#7662=DIRECTION('center_axis',(0.,0.707106781186548,-0.707106781186548));
#7663=DIRECTION('ref_axis',(-1.,0.,0.));
#7664=DIRECTION('',(1.,0.,0.));
#7665=DIRECTION('center_axis',(0.,1.,0.));
#7666=DIRECTION('ref_axis',(-1.,0.,0.));
#7667=DIRECTION('axis',(0.,0.,1.));
#7668=DIRECTION('refdir',(1.,0.,0.));
#7669=DIRECTION('center_axis',(0.,1.,0.));
#7670=DIRECTION('ref_axis',(1.,0.,0.));
#7671=DIRECTION('center_axis',(0.,1.,0.));
#7672=DIRECTION('ref_axis',(1.,0.,0.));
#7673=DIRECTION('',(0.707106781186548,-0.707106781186547,-8.65956056235494E-17));
#7674=DIRECTION('center_axis',(0.,-1.,0.));
#7675=DIRECTION('ref_axis',(1.,0.,0.));
#7676=DIRECTION('center_axis',(0.,1.,0.));
#7677=DIRECTION('ref_axis',(1.,0.,0.));
#7678=DIRECTION('',(0.,-1.,0.));
#7679=DIRECTION('center_axis',(0.,-1.,0.));
#7680=DIRECTION('ref_axis',(1.,0.,0.));
#7681=DIRECTION('center_axis',(0.,1.,0.));
#7682=DIRECTION('ref_axis',(1.,0.,0.));
#7683=DIRECTION('center_axis',(0.,1.,0.));
#7684=DIRECTION('ref_axis',(1.,0.,0.));
#7685=DIRECTION('center_axis',(0.,1.,0.));
#7686=DIRECTION('ref_axis',(1.,0.,0.));
#7687=DIRECTION('',(0.,-1.,0.));
#7688=DIRECTION('center_axis',(0.,1.,0.));
#7689=DIRECTION('ref_axis',(1.,0.,0.));
#7690=DIRECTION('center_axis',(0.,1.,0.));
#7691=DIRECTION('ref_axis',(1.,0.,0.));
#7692=DIRECTION('axis',(0.,0.,1.));
#7693=DIRECTION('refdir',(1.,0.,0.));
#7694=DIRECTION('center_axis',(0.866025403784439,0.,-0.5));
#7695=DIRECTION('ref_axis',(0.5,0.,0.866025403784439));
#7696=DIRECTION('',(-0.5,0.,-0.866025403784439));
#7697=DIRECTION('',(0.,-1.,0.));
#7698=DIRECTION('',(0.5,0.,0.866025403784439));
#7699=DIRECTION('',(0.,-1.,0.));
#7700=DIRECTION('center_axis',(1.20185167898973E-16,0.,-1.));
#7701=DIRECTION('ref_axis',(1.,0.,1.20185167898973E-16));
#7702=DIRECTION('',(-1.,0.,-1.20185167898973E-16));
#7703=DIRECTION('',(0.,-1.,0.));
#7704=DIRECTION('',(1.,0.,1.20185167898973E-16));
#7705=DIRECTION('center_axis',(-0.866025403784439,0.,-0.5));
#7706=DIRECTION('ref_axis',(0.5,0.,-0.866025403784439));
#7707=DIRECTION('',(-0.5,0.,0.866025403784439));
#7708=DIRECTION('',(0.,-1.,0.));
#7709=DIRECTION('',(0.5,0.,-0.866025403784439));
#7710=DIRECTION('center_axis',(-0.866025403784439,0.,0.5));
#7711=DIRECTION('ref_axis',(-0.5,0.,-0.866025403784439));
#7712=DIRECTION('',(0.5,0.,0.866025403784439));
#7713=DIRECTION('',(0.,-1.,0.));
#7714=DIRECTION('',(-0.5,0.,-0.866025403784439));
#7715=DIRECTION('center_axis',(-2.40370335797945E-16,0.,1.));
#7716=DIRECTION('ref_axis',(-1.,0.,-2.40370335797945E-16));
#7717=DIRECTION('',(1.,0.,2.40370335797945E-16));
#7718=DIRECTION('',(0.,-1.,0.));
#7719=DIRECTION('',(-1.,0.,-2.40370335797945E-16));
#7720=DIRECTION('center_axis',(0.866025403784439,0.,0.5));
#7721=DIRECTION('ref_axis',(-0.5,0.,0.866025403784439));
#7722=DIRECTION('',(0.5,0.,-0.866025403784439));
#7723=DIRECTION('',(-0.5,0.,0.866025403784439));
#7724=DIRECTION('center_axis',(0.,1.,0.));
#7725=DIRECTION('ref_axis',(1.,0.,0.));
#7726=DIRECTION('center_axis',(0.,-1.,0.));
#7727=DIRECTION('ref_axis',(0.,0.,-1.));
#7728=DIRECTION('center_axis',(0.,1.,0.));
#7729=DIRECTION('ref_axis',(1.,0.,0.));
#7730=DIRECTION('center_axis',(0.,1.,0.));
#7731=DIRECTION('ref_axis',(1.,0.,0.));
#7732=DIRECTION('center_axis',(0.,1.,0.));
#7733=DIRECTION('ref_axis',(0.,0.,1.));
#7734=DIRECTION('center_axis',(0.,-1.,0.));
#7735=DIRECTION('ref_axis',(1.,0.,0.));
#7736=DIRECTION('center_axis',(0.,-1.,0.));
#7737=DIRECTION('ref_axis',(1.,0.,0.));
#7738=DIRECTION('center_axis',(0.,-1.,0.));
#7739=DIRECTION('ref_axis',(1.,0.,0.));
#7740=DIRECTION('',(0.707106781186548,0.707106781186547,8.65956056235493E-17));
#7741=DIRECTION('center_axis',(0.,-1.,0.));
#7742=DIRECTION('ref_axis',(1.,0.,0.));
#7743=DIRECTION('center_axis',(0.,-1.,0.));
#7744=DIRECTION('ref_axis',(1.,0.,0.));
#7745=DIRECTION('',(0.,1.,0.));
#7746=DIRECTION('center_axis',(0.,1.,0.));
#7747=DIRECTION('ref_axis',(1.,0.,0.));
#7748=DIRECTION('center_axis',(0.,-1.,0.));
#7749=DIRECTION('ref_axis',(1.,0.,0.));
#7750=DIRECTION('',(-0.707106781186547,0.707106781186548,-8.65956056235493E-17));
#7751=DIRECTION('center_axis',(0.,-1.,0.));
#7752=DIRECTION('ref_axis',(0.,0.,-1.));
#7753=DIRECTION('center_axis',(0.,-1.,0.));
#7754=DIRECTION('ref_axis',(1.,0.,0.));
#7755=DIRECTION('center_axis',(0.,1.,0.));
#7756=DIRECTION('ref_axis',(1.,0.,0.));
#7757=DIRECTION('center_axis',(0.,1.,0.));
#7758=DIRECTION('ref_axis',(1.,0.,0.));
#7759=DIRECTION('',(-0.447213595499958,0.894427190999916,-5.47678698264203E-17));
#7760=DIRECTION('center_axis',(0.,-1.,0.));
#7761=DIRECTION('ref_axis',(1.,0.,0.));
#7762=DIRECTION('',(0.,1.,0.));
#7763=DIRECTION('axis',(0.,0.,1.));
#7764=DIRECTION('refdir',(1.,0.,0.));
#7765=DIRECTION('center_axis',(0.,1.,0.));
#7766=DIRECTION('ref_axis',(1.,0.,0.));
#7767=DIRECTION('center_axis',(0.,1.,0.));
#7768=DIRECTION('ref_axis',(1.,0.,0.));
#7769=DIRECTION('',(0.707106781186547,-0.707106781186548,-8.65956056235493E-17));
#7770=DIRECTION('center_axis',(0.,-1.,0.));
#7771=DIRECTION('ref_axis',(1.,0.,0.));
#7772=DIRECTION('center_axis',(0.,1.,0.));
#7773=DIRECTION('ref_axis',(1.,0.,0.));
#7774=DIRECTION('',(0.,-1.,0.));
#7775=DIRECTION('center_axis',(0.,-1.,0.));
#7776=DIRECTION('ref_axis',(1.,0.,0.));
#7777=DIRECTION('center_axis',(0.,1.,0.));
#7778=DIRECTION('ref_axis',(1.,0.,0.));
#7779=DIRECTION('center_axis',(0.,1.,0.));
#7780=DIRECTION('ref_axis',(1.,0.,0.));
#7781=DIRECTION('center_axis',(0.,1.,0.));
#7782=DIRECTION('ref_axis',(1.,0.,0.));
#7783=DIRECTION('',(0.,-1.,0.));
#7784=DIRECTION('center_axis',(0.,1.,0.));
#7785=DIRECTION('ref_axis',(1.,0.,0.));
#7786=DIRECTION('center_axis',(0.,1.,0.));
#7787=DIRECTION('ref_axis',(1.,0.,0.));
#7788=DIRECTION('axis',(0.,0.,1.));
#7789=DIRECTION('refdir',(1.,0.,0.));
#7790=DIRECTION('center_axis',(0.,1.,0.));
#7791=DIRECTION('ref_axis',(0.,0.,1.));
#7792=DIRECTION('center_axis',(0.,-1.,0.));
#7793=DIRECTION('ref_axis',(1.,0.,0.));
#7794=DIRECTION('center_axis',(0.,-1.,0.));
#7795=DIRECTION('ref_axis',(1.,0.,0.));
#7796=DIRECTION('center_axis',(0.,-1.,0.));
#7797=DIRECTION('ref_axis',(1.,0.,0.));
#7798=DIRECTION('',(0.707106781186547,0.707106781186548,8.65956056235493E-17));
#7799=DIRECTION('center_axis',(0.,-1.,0.));
#7800=DIRECTION('ref_axis',(1.,0.,0.));
#7801=DIRECTION('center_axis',(0.,-1.,0.));
#7802=DIRECTION('ref_axis',(1.,0.,0.));
#7803=DIRECTION('',(0.,1.,0.));
#7804=DIRECTION('center_axis',(0.,1.,0.));
#7805=DIRECTION('ref_axis',(1.,0.,0.));
#7806=DIRECTION('center_axis',(0.,-1.,0.));
#7807=DIRECTION('ref_axis',(1.,0.,0.));
#7808=DIRECTION('',(-0.707106781186547,0.707106781186548,-8.65956056235493E-17));
#7809=DIRECTION('center_axis',(0.,-1.,0.));
#7810=DIRECTION('ref_axis',(0.,0.,-1.));
#7811=DIRECTION('center_axis',(0.,-1.,0.));
#7812=DIRECTION('ref_axis',(1.,0.,0.));
#7813=DIRECTION('center_axis',(0.,1.,0.));
#7814=DIRECTION('ref_axis',(1.,0.,0.));
#7815=DIRECTION('center_axis',(0.,1.,0.));
#7816=DIRECTION('ref_axis',(1.,0.,0.));
#7817=DIRECTION('',(-0.447213595499958,0.894427190999916,-5.47678698264203E-17));
#7818=DIRECTION('center_axis',(0.,-1.,0.));
#7819=DIRECTION('ref_axis',(1.,0.,0.));
#7820=DIRECTION('center_axis',(0.,1.,0.));
#7821=DIRECTION('ref_axis',(1.,0.,0.));
#7822=DIRECTION('',(0.,1.,0.));
#7823=DIRECTION('center_axis',(0.,1.,0.));
#7824=DIRECTION('ref_axis',(1.,0.,0.));
#7825=DIRECTION('center_axis',(0.,-1.,0.));
#7826=DIRECTION('ref_axis',(1.,0.,0.));
#7827=DIRECTION('',(-0.707106781186547,0.707106781186548,-8.65956056235493E-17));
#7828=DIRECTION('center_axis',(0.,-1.,0.));
#7829=DIRECTION('ref_axis',(0.,0.,-1.));
#7830=DIRECTION('center_axis',(0.866025403784439,0.,-0.5));
#7831=DIRECTION('ref_axis',(0.5,0.,0.866025403784439));
#7832=DIRECTION('',(-0.5,0.,-0.866025403784439));
#7833=DIRECTION('',(0.,-1.,0.));
#7834=DIRECTION('',(0.5,0.,0.866025403784439));
#7835=DIRECTION('',(0.,-1.,0.));
#7836=DIRECTION('center_axis',(1.60246890531964E-16,0.,-1.));
#7837=DIRECTION('ref_axis',(1.,0.,1.60246890531964E-16));
#7838=DIRECTION('',(-1.,0.,-1.60246890531964E-16));
#7839=DIRECTION('',(0.,-1.,0.));
#7840=DIRECTION('',(1.,0.,1.60246890531964E-16));
#7841=DIRECTION('center_axis',(-0.866025403784439,0.,-0.5));
#7842=DIRECTION('ref_axis',(0.5,0.,-0.866025403784439));
#7843=DIRECTION('',(-0.5,0.,0.866025403784439));
#7844=DIRECTION('',(0.,-1.,0.));
#7845=DIRECTION('',(0.5,0.,-0.866025403784439));
#7846=DIRECTION('center_axis',(-0.866025403784439,0.,0.5));
#7847=DIRECTION('ref_axis',(-0.5,0.,-0.866025403784439));
#7848=DIRECTION('',(0.5,0.,0.866025403784439));
#7849=DIRECTION('',(0.,-1.,0.));
#7850=DIRECTION('',(-0.5,0.,-0.866025403784439));
#7851=DIRECTION('center_axis',(-1.60246890531964E-16,0.,1.));
#7852=DIRECTION('ref_axis',(-1.,0.,-1.60246890531964E-16));
#7853=DIRECTION('',(1.,0.,1.60246890531964E-16));
#7854=DIRECTION('',(0.,-1.,0.));
#7855=DIRECTION('',(-1.,0.,-1.60246890531964E-16));
#7856=DIRECTION('center_axis',(0.866025403784439,0.,0.5));
#7857=DIRECTION('ref_axis',(-0.5,0.,0.866025403784439));
#7858=DIRECTION('',(0.5,0.,-0.866025403784439));
#7859=DIRECTION('',(-0.5,0.,0.866025403784439));
#7860=DIRECTION('center_axis',(0.,1.,0.));
#7861=DIRECTION('ref_axis',(1.,0.,0.));
#7862=DIRECTION('center_axis',(0.,-1.,0.));
#7863=DIRECTION('ref_axis',(0.,0.,-1.));
#7864=DIRECTION('',(0.,0.,1.));
#7865=DIRECTION('',(1.,0.,0.));
#7866=DIRECTION('',(0.,0.,1.));
#7867=DIRECTION('',(1.,0.,0.));
#7868=DIRECTION('',(0.,0.,1.));
#7869=DIRECTION('',(1.,0.,0.));
#7870=DIRECTION('',(0.,0.,1.));
#7871=DIRECTION('',(1.,0.,0.));
#7872=DIRECTION('',(0.,0.,1.));
#7873=DIRECTION('',(1.,0.,0.));
#7874=DIRECTION('',(0.,0.,1.));
#7875=DIRECTION('',(1.,0.,0.));
#7876=DIRECTION('',(0.,0.,1.));
#7877=DIRECTION('',(1.,0.,0.));
#7878=DIRECTION('',(0.,0.,1.));
#7879=DIRECTION('',(1.,0.,0.));
#7880=DIRECTION('',(0.,0.,1.));
#7881=DIRECTION('',(1.,0.,0.));
#7882=DIRECTION('',(0.,0.,1.));
#7883=DIRECTION('',(1.,0.,0.));
#7884=DIRECTION('',(0.,0.,1.));
#7885=DIRECTION('',(1.,0.,0.));
#7886=DIRECTION('',(0.,0.,1.));
#7887=DIRECTION('',(1.,0.,0.));
#7888=DIRECTION('',(0.,0.,1.));
#7889=DIRECTION('',(1.,0.,0.));
#7890=DIRECTION('',(-1.,0.,2.22044604925031E-16));
#7891=DIRECTION('',(2.22044604925031E-16,0.,1.));
#7892=DIRECTION('',(0.,1.,2.22044604925031E-16));
#7893=DIRECTION('',(1.,0.,0.));
#7894=DIRECTION('',(0.,1.,2.22044604925031E-16));
#7895=DIRECTION('',(1.,0.,0.));
#7896=DIRECTION('',(-1.,0.,2.22044604925031E-16));
#7897=DIRECTION('',(2.22044604925031E-16,0.,1.));
#7898=DIRECTION('',(0.,1.,2.22044604925031E-16));
#7899=DIRECTION('',(1.,0.,0.));
#7900=DIRECTION('',(0.,1.,2.22044604925031E-16));
#7901=DIRECTION('',(1.,0.,0.));
#7902=DIRECTION('',(-1.,0.,2.22044604925031E-16));
#7903=DIRECTION('',(2.22044604925031E-16,0.,1.));
#7904=DIRECTION('',(0.,1.,2.22044604925031E-16));
#7905=DIRECTION('',(1.,0.,0.));
#7906=DIRECTION('',(0.,1.,2.22044604925031E-16));
#7907=DIRECTION('',(1.,0.,0.));
#7908=DIRECTION('',(-1.,0.,2.22044604925031E-16));
#7909=DIRECTION('',(2.22044604925031E-16,0.,1.));
#7910=DIRECTION('',(0.,1.,2.22044604925031E-16));
#7911=DIRECTION('',(1.,0.,0.));
#7912=DIRECTION('',(0.,1.,2.22044604925031E-16));
#7913=DIRECTION('',(1.,0.,0.));
#7914=DIRECTION('',(0.,0.,1.));
#7915=DIRECTION('',(1.,0.,0.));
#7916=DIRECTION('',(0.,0.,1.));
#7917=DIRECTION('',(2.22044604925031E-16,1.,0.));
#7918=DIRECTION('',(0.,0.,1.));
#7919=DIRECTION('',(2.22044604925031E-16,1.,0.));
#7920=DIRECTION('',(0.,0.,1.));
#7921=DIRECTION('',(2.22044604925031E-16,-1.,0.));
#7922=DIRECTION('',(0.,0.,1.));
#7923=DIRECTION('',(2.22044604925031E-16,-1.,0.));
#7924=DIRECTION('',(0.,0.,1.));
#7925=DIRECTION('',(1.,0.,0.));
#7926=DIRECTION('',(0.,0.,1.));
#7927=DIRECTION('',(2.22044604925031E-16,1.,0.));
#7928=DIRECTION('',(0.,0.,1.));
#7929=DIRECTION('',(2.22044604925031E-16,1.,0.));
#7930=DIRECTION('',(0.,0.,1.));
#7931=DIRECTION('',(2.22044604925031E-16,-1.,0.));
#7932=DIRECTION('',(0.,0.,1.));
#7933=DIRECTION('',(2.22044604925031E-16,-1.,0.));
#7934=DIRECTION('',(0.,0.,1.));
#7935=DIRECTION('',(1.,0.,0.));
#7936=DIRECTION('',(0.,0.,1.));
#7937=DIRECTION('',(2.22044604925031E-16,1.,0.));
#7938=DIRECTION('',(0.,0.,1.));
#7939=DIRECTION('',(2.22044604925031E-16,1.,0.));
#7940=DIRECTION('',(0.,0.,1.));
#7941=DIRECTION('',(2.22044604925031E-16,-1.,0.));
#7942=DIRECTION('',(0.,0.,1.));
#7943=DIRECTION('',(2.22044604925031E-16,-1.,0.));
#7944=DIRECTION('',(0.,0.,1.));
#7945=DIRECTION('',(1.,0.,0.));
#7946=DIRECTION('',(0.,0.,1.));
#7947=DIRECTION('',(2.22044604925031E-16,1.,0.));
#7948=DIRECTION('',(0.,0.,1.));
#7949=DIRECTION('',(2.22044604925031E-16,1.,0.));
#7950=DIRECTION('',(0.,0.,1.));
#7951=DIRECTION('',(2.22044604925031E-16,-1.,0.));
#7952=DIRECTION('',(0.,0.,1.));
#7953=DIRECTION('',(2.22044604925031E-16,-1.,0.));
#7954=DIRECTION('',(0.,0.,1.));
#7955=DIRECTION('',(2.22044604925031E-16,1.,0.));
#7956=DIRECTION('',(0.,0.,1.));
#7957=DIRECTION('',(-1.,1.22464679914735E-16,0.));
#7958=DIRECTION('',(0.,0.,1.));
#7959=DIRECTION('',(-1.,1.22464679914735E-16,0.));
#7960=DIRECTION('',(0.,0.,1.));
#7961=DIRECTION('',(1.,0.,0.));
#7962=DIRECTION('',(0.,0.,1.));
#7963=DIRECTION('',(1.,0.,0.));
#7964=DIRECTION('',(0.,0.,1.));
#7965=DIRECTION('',(2.22044604925031E-16,1.,0.));
#7966=DIRECTION('',(0.,0.,1.));
#7967=DIRECTION('',(-1.,1.22464679914735E-16,0.));
#7968=DIRECTION('',(0.,0.,1.));
#7969=DIRECTION('',(-1.,1.22464679914735E-16,0.));
#7970=DIRECTION('',(0.,0.,1.));
#7971=DIRECTION('',(1.,0.,0.));
#7972=DIRECTION('',(0.,0.,1.));
#7973=DIRECTION('',(1.,0.,0.));
#7974=DIRECTION('',(0.,0.,1.));
#7975=DIRECTION('',(2.22044604925031E-16,1.,0.));
#7976=DIRECTION('',(0.,0.,1.));
#7977=DIRECTION('',(-1.,1.22464679914735E-16,0.));
#7978=DIRECTION('',(0.,0.,1.));
#7979=DIRECTION('',(-1.,1.22464679914735E-16,0.));
#7980=DIRECTION('',(0.,0.,1.));
#7981=DIRECTION('',(1.,0.,0.));
#7982=DIRECTION('',(0.,0.,1.));
#7983=DIRECTION('',(1.,0.,0.));
#7984=DIRECTION('',(0.,0.,1.));
#7985=DIRECTION('',(2.22044604925031E-16,1.,0.));
#7986=DIRECTION('',(0.,0.,1.));
#7987=DIRECTION('',(-1.,1.22464679914735E-16,0.));
#7988=DIRECTION('',(0.,0.,1.));
#7989=DIRECTION('',(-1.,1.22464679914735E-16,0.));
#7990=DIRECTION('',(0.,0.,1.));
#7991=DIRECTION('',(1.,0.,0.));
#7992=DIRECTION('',(0.,0.,1.));
#7993=DIRECTION('',(1.,0.,0.));
#7994=DIRECTION('',(0.,-1.,2.22044604925031E-16));
#7995=DIRECTION('',(1.,0.,0.));
#7996=DIRECTION('',(0.,-1.,2.22044604925031E-16));
#7997=DIRECTION('',(1.,0.,0.));
#7998=DIRECTION('',(0.,-1.,2.22044604925031E-16));
#7999=DIRECTION('',(1.,0.,0.));
#8000=DIRECTION('',(0.,-1.,2.22044604925031E-16));
#8001=DIRECTION('',(1.,0.,0.));
#8002=DIRECTION('',(0.,0.,1.));
#8003=DIRECTION('',(2.22044604925031E-16,1.,0.));
#8004=DIRECTION('',(0.,-1.,2.22044604925031E-16));
#8005=DIRECTION('',(1.,0.,0.));
#8006=DIRECTION('',(0.,-1.,2.22044604925031E-16));
#8007=DIRECTION('',(1.,0.,0.));
#8008=DIRECTION('',(0.,0.,1.));
#8009=DIRECTION('',(2.22044604925031E-16,1.,0.));
#8010=DIRECTION('',(0.,-1.,2.22044604925031E-16));
#8011=DIRECTION('',(1.,0.,0.));
#8012=DIRECTION('',(0.,-1.,2.22044604925031E-16));
#8013=DIRECTION('',(1.,0.,0.));
#8014=DIRECTION('',(0.,0.,1.));
#8015=DIRECTION('',(2.22044604925031E-16,1.,0.));
#8016=DIRECTION('',(0.,-1.,2.22044604925031E-16));
#8017=DIRECTION('',(1.,0.,0.));
#8018=DIRECTION('',(0.,-1.,2.22044604925031E-16));
#8019=DIRECTION('',(1.,0.,0.));
#8020=DIRECTION('',(0.,0.,1.));
#8021=DIRECTION('',(2.22044604925031E-16,1.,0.));
#8022=DIRECTION('',(0.,-1.,2.22044604925031E-16));
#8023=DIRECTION('',(1.,0.,0.));
#8024=DIRECTION('',(0.,-1.,2.22044604925031E-16));
#8025=DIRECTION('',(1.,0.,0.));
#8026=DIRECTION('',(0.,1.,0.));
#8027=DIRECTION('',(1.,0.,0.));
#8028=DIRECTION('',(0.,0.,1.));
#8029=DIRECTION('',(1.,0.,0.));
#8030=DIRECTION('',(0.,0.,1.));
#8031=DIRECTION('',(1.,0.,0.));
#8032=DIRECTION('',(0.,1.,0.));
#8033=DIRECTION('',(1.,0.,0.));
#8034=DIRECTION('',(0.,0.,1.));
#8035=DIRECTION('',(1.,0.,0.));
#8036=DIRECTION('',(0.,0.,1.));
#8037=DIRECTION('',(1.,0.,0.));
#8038=DIRECTION('',(0.,1.,0.));
#8039=DIRECTION('',(1.,0.,0.));
#8040=DIRECTION('',(0.,0.,1.));
#8041=DIRECTION('',(1.,0.,0.));
#8042=DIRECTION('',(0.,0.,1.));
#8043=DIRECTION('',(1.,0.,0.));
#8044=DIRECTION('',(0.,1.,0.));
#8045=DIRECTION('',(1.,0.,0.));
#8046=DIRECTION('',(0.,0.,1.));
#8047=DIRECTION('',(1.,0.,0.));
#8048=DIRECTION('',(0.,0.,1.));
#8049=DIRECTION('',(1.,0.,0.));
#8050=DIRECTION('',(0.,-1.,2.22044604925031E-16));
#8051=DIRECTION('',(1.,0.,0.));
#8052=DIRECTION('',(0.,-1.,2.22044604925031E-16));
#8053=DIRECTION('',(1.,0.,0.));
#8054=DIRECTION('',(0.,-1.,2.22044604925031E-16));
#8055=DIRECTION('',(1.,0.,0.));
#8056=DIRECTION('',(0.,-1.,2.22044604925031E-16));
#8057=DIRECTION('',(1.,0.,0.));
#8058=CARTESIAN_POINT('',(0.,0.,0.));
#8059=CARTESIAN_POINT('',(0.,0.,0.));
#8060=CARTESIAN_POINT('Origin',(-19.,-19.,-0.8));
#8061=CARTESIAN_POINT('',(-19.275,-19.,0.));
#8062=CARTESIAN_POINT('Origin',(-19.,-19.,0.));
#8063=CARTESIAN_POINT('',(-19.275,-19.,-0.8));
#8064=CARTESIAN_POINT('',(-19.275,-19.,-0.8));
#8065=CARTESIAN_POINT('Origin',(-19.,-19.,-0.8));
#8066=CARTESIAN_POINT('Origin',(-19.,-19.,-0.8));
#8067=CARTESIAN_POINT('',(-21.,-19.,0.));
#8068=CARTESIAN_POINT('Origin',(-19.,-19.,0.));
#8069=CARTESIAN_POINT('',(-21.,-19.,-0.8));
#8070=CARTESIAN_POINT('',(-21.,-19.,-0.8));
#8071=CARTESIAN_POINT('Origin',(-19.,-19.,-0.8));
#8072=CARTESIAN_POINT('Origin',(-19.,-19.,0.));
#8073=CARTESIAN_POINT('Origin',(-19.,-19.,-0.8));
#8074=CARTESIAN_POINT('',(0.,0.,0.));
#8075=CARTESIAN_POINT('Origin',(-19.,-19.,-1.6));
#8076=CARTESIAN_POINT('',(-19.6,-19.,-0.8));
#8077=CARTESIAN_POINT('Origin',(-19.,-19.,-0.8));
#8078=CARTESIAN_POINT('',(-19.6,-19.,-1.6));
#8079=CARTESIAN_POINT('',(-19.6,-19.,-1.6));
#8080=CARTESIAN_POINT('Origin',(-19.,-19.,-1.6));
#8081=CARTESIAN_POINT('Origin',(-19.,-19.,-1.6));
#8082=CARTESIAN_POINT('',(-21.,-19.,-0.8));
#8083=CARTESIAN_POINT('Origin',(-19.,-19.,-0.8));
#8084=CARTESIAN_POINT('',(-21.,-19.,-1.6));
#8085=CARTESIAN_POINT('',(-21.,-19.,-1.6));
#8086=CARTESIAN_POINT('Origin',(-19.,-19.,-1.6));
#8087=CARTESIAN_POINT('Origin',(-19.,-19.,-0.8));
#8088=CARTESIAN_POINT('Origin',(-19.,-19.,-1.6));
#8089=CARTESIAN_POINT('',(0.,0.,0.));
#8090=CARTESIAN_POINT('Origin',(-19.,19.,-0.8));
#8091=CARTESIAN_POINT('',(-19.275,19.,0.));
#8092=CARTESIAN_POINT('Origin',(-19.,19.,0.));
#8093=CARTESIAN_POINT('',(-19.275,19.,-0.8));
#8094=CARTESIAN_POINT('',(-19.275,19.,-0.8));
#8095=CARTESIAN_POINT('Origin',(-19.,19.,-0.8));
#8096=CARTESIAN_POINT('Origin',(-19.,19.,-0.8));
#8097=CARTESIAN_POINT('',(-21.,19.,0.));
#8098=CARTESIAN_POINT('Origin',(-19.,19.,0.));
#8099=CARTESIAN_POINT('',(-21.,19.,-0.8));
#8100=CARTESIAN_POINT('',(-21.,19.,-0.8));
#8101=CARTESIAN_POINT('Origin',(-19.,19.,-0.8));
#8102=CARTESIAN_POINT('Origin',(-19.,19.,0.));
#8103=CARTESIAN_POINT('Origin',(-19.,19.,-0.8));
#8104=CARTESIAN_POINT('',(0.,0.,0.));
#8105=CARTESIAN_POINT('Origin',(-19.,19.,-1.6));
#8106=CARTESIAN_POINT('',(-19.6,19.,-0.8));
#8107=CARTESIAN_POINT('Origin',(-19.,19.,-0.8));
#8108=CARTESIAN_POINT('',(-19.6,19.,-1.6));
#8109=CARTESIAN_POINT('',(-19.6,19.,-1.6));
#8110=CARTESIAN_POINT('Origin',(-19.,19.,-1.6));
#8111=CARTESIAN_POINT('Origin',(-19.,19.,-1.6));
#8112=CARTESIAN_POINT('',(-21.,19.,-0.8));
#8113=CARTESIAN_POINT('Origin',(-19.,19.,-0.8));
#8114=CARTESIAN_POINT('',(-21.,19.,-1.6));
#8115=CARTESIAN_POINT('',(-21.,19.,-1.6));
#8116=CARTESIAN_POINT('Origin',(-19.,19.,-1.6));
#8117=CARTESIAN_POINT('Origin',(-19.,19.,-0.8));
#8118=CARTESIAN_POINT('Origin',(-19.,19.,-1.6));
#8119=CARTESIAN_POINT('',(0.,0.,0.));
#8120=CARTESIAN_POINT('Origin',(19.,-19.,-0.8));
#8121=CARTESIAN_POINT('',(18.725,-19.,0.));
#8122=CARTESIAN_POINT('Origin',(19.,-19.,0.));
#8123=CARTESIAN_POINT('',(18.725,-19.,-0.8));
#8124=CARTESIAN_POINT('',(18.725,-19.,-0.8));
#8125=CARTESIAN_POINT('Origin',(19.,-19.,-0.8));
#8126=CARTESIAN_POINT('Origin',(19.,-19.,-0.8));
#8127=CARTESIAN_POINT('',(17.,-19.,0.));
#8128=CARTESIAN_POINT('Origin',(19.,-19.,0.));
#8129=CARTESIAN_POINT('',(17.,-19.,-0.8));
#8130=CARTESIAN_POINT('',(17.,-19.,-0.8));
#8131=CARTESIAN_POINT('Origin',(19.,-19.,-0.8));
#8132=CARTESIAN_POINT('Origin',(19.,-19.,0.));
#8133=CARTESIAN_POINT('Origin',(19.,-19.,-0.8));
#8134=CARTESIAN_POINT('',(0.,0.,0.));
#8135=CARTESIAN_POINT('Origin',(19.,-19.,-1.6));
#8136=CARTESIAN_POINT('',(18.4,-19.,-0.8));
#8137=CARTESIAN_POINT('Origin',(19.,-19.,-0.8));
#8138=CARTESIAN_POINT('',(18.4,-19.,-1.6));
#8139=CARTESIAN_POINT('',(18.4,-19.,-1.6));
#8140=CARTESIAN_POINT('Origin',(19.,-19.,-1.6));
#8141=CARTESIAN_POINT('Origin',(19.,-19.,-1.6));
#8142=CARTESIAN_POINT('',(17.,-19.,-0.8));
#8143=CARTESIAN_POINT('Origin',(19.,-19.,-0.8));
#8144=CARTESIAN_POINT('',(17.,-19.,-1.6));
#8145=CARTESIAN_POINT('',(17.,-19.,-1.6));
#8146=CARTESIAN_POINT('Origin',(19.,-19.,-1.6));
#8147=CARTESIAN_POINT('Origin',(19.,-19.,-0.8));
#8148=CARTESIAN_POINT('Origin',(19.,-19.,-1.6));
#8149=CARTESIAN_POINT('',(0.,0.,0.));
#8150=CARTESIAN_POINT('Origin',(19.,19.,-0.8));
#8151=CARTESIAN_POINT('',(18.725,19.,0.));
#8152=CARTESIAN_POINT('Origin',(19.,19.,0.));
#8153=CARTESIAN_POINT('',(18.725,19.,-0.8));
#8154=CARTESIAN_POINT('',(18.725,19.,-0.8));
#8155=CARTESIAN_POINT('Origin',(19.,19.,-0.8));
#8156=CARTESIAN_POINT('Origin',(19.,19.,-0.8));
#8157=CARTESIAN_POINT('',(17.,19.,0.));
#8158=CARTESIAN_POINT('Origin',(19.,19.,0.));
#8159=CARTESIAN_POINT('',(17.,19.,-0.8));
#8160=CARTESIAN_POINT('',(17.,19.,-0.8));
#8161=CARTESIAN_POINT('Origin',(19.,19.,-0.8));
#8162=CARTESIAN_POINT('Origin',(19.,19.,0.));
#8163=CARTESIAN_POINT('Origin',(19.,19.,-0.8));
#8164=CARTESIAN_POINT('',(0.,0.,0.));
#8165=CARTESIAN_POINT('Origin',(19.,19.,-1.6));
#8166=CARTESIAN_POINT('',(18.4,19.,-0.8));
#8167=CARTESIAN_POINT('Origin',(19.,19.,-0.8));
#8168=CARTESIAN_POINT('',(18.4,19.,-1.6));
#8169=CARTESIAN_POINT('',(18.4,19.,-1.6));
#8170=CARTESIAN_POINT('Origin',(19.,19.,-1.6));
#8171=CARTESIAN_POINT('Origin',(19.,19.,-1.6));
#8172=CARTESIAN_POINT('',(17.,19.,-0.8));
#8173=CARTESIAN_POINT('Origin',(19.,19.,-0.8));
#8174=CARTESIAN_POINT('',(17.,19.,-1.6));
#8175=CARTESIAN_POINT('',(17.,19.,-1.6));
#8176=CARTESIAN_POINT('Origin',(19.,19.,-1.6));
#8177=CARTESIAN_POINT('Origin',(19.,19.,-0.8));
#8178=CARTESIAN_POINT('Origin',(19.,19.,-1.6));
#8179=CARTESIAN_POINT('',(0.,0.,0.));
#8180=CARTESIAN_POINT('Origin',(19.,-19.,40.7));
#8181=CARTESIAN_POINT('',(18.5,-19.,40.7));
#8182=CARTESIAN_POINT('Origin',(19.,-19.,40.7));
#8183=CARTESIAN_POINT('',(18.5,-19.,41.2));
#8184=CARTESIAN_POINT('',(18.5,-19.,40.7));
#8185=CARTESIAN_POINT('Origin',(19.,-19.,41.2));
#8186=CARTESIAN_POINT('Origin',(19.,-19.,40.7));
#8187=CARTESIAN_POINT('',(18.725,-19.,40.7));
#8188=CARTESIAN_POINT('Origin',(19.,-19.,40.7));
#8189=CARTESIAN_POINT('Origin',(-19.,19.,40.7));
#8190=CARTESIAN_POINT('',(-19.5,19.,40.7));
#8191=CARTESIAN_POINT('Origin',(-19.,19.,40.7));
#8192=CARTESIAN_POINT('',(-19.5,19.,41.2));
#8193=CARTESIAN_POINT('',(-19.5,19.,40.7));
#8194=CARTESIAN_POINT('Origin',(-19.,19.,41.2));
#8195=CARTESIAN_POINT('Origin',(-19.,19.,40.7));
#8196=CARTESIAN_POINT('',(-19.275,19.,40.7));
#8197=CARTESIAN_POINT('Origin',(-19.,19.,40.7));
#8198=CARTESIAN_POINT('Origin',(-19.,-19.,40.7));
#8199=CARTESIAN_POINT('',(-19.5,-19.,40.7));
#8200=CARTESIAN_POINT('Origin',(-19.,-19.,40.7));
#8201=CARTESIAN_POINT('',(-19.5,-19.,41.2));
#8202=CARTESIAN_POINT('',(-19.5,-19.,40.7));
#8203=CARTESIAN_POINT('Origin',(-19.,-19.,41.2));
#8204=CARTESIAN_POINT('Origin',(-19.,-19.,40.7));
#8205=CARTESIAN_POINT('',(-19.275,-19.,40.7));
#8206=CARTESIAN_POINT('Origin',(-19.,-19.,40.7));
#8207=CARTESIAN_POINT('Origin',(19.,19.,40.7));
#8208=CARTESIAN_POINT('',(18.5,19.,40.7));
#8209=CARTESIAN_POINT('Origin',(19.,19.,40.7));
#8210=CARTESIAN_POINT('',(18.5,19.,41.2));
#8211=CARTESIAN_POINT('',(18.5,19.,40.7));
#8212=CARTESIAN_POINT('Origin',(19.,19.,41.2));
#8213=CARTESIAN_POINT('Origin',(19.,19.,40.7));
#8214=CARTESIAN_POINT('',(18.725,19.,40.7));
#8215=CARTESIAN_POINT('Origin',(19.,19.,40.7));
#8216=CARTESIAN_POINT('Origin',(19.,-19.,39.9));
#8217=CARTESIAN_POINT('',(18.725,-19.,40.));
#8218=CARTESIAN_POINT('Origin',(19.,-19.,40.));
#8219=CARTESIAN_POINT('',(18.725,-19.,39.9));
#8220=CARTESIAN_POINT('Origin',(-19.,19.,39.9));
#8221=CARTESIAN_POINT('',(-19.275,19.,40.));
#8222=CARTESIAN_POINT('Origin',(-19.,19.,40.));
#8223=CARTESIAN_POINT('',(-19.275,19.,39.9));
#8224=CARTESIAN_POINT('Origin',(-19.,-19.,39.9));
#8225=CARTESIAN_POINT('',(-19.275,-19.,40.));
#8226=CARTESIAN_POINT('Origin',(-19.,-19.,40.));
#8227=CARTESIAN_POINT('',(-19.275,-19.,39.9));
#8228=CARTESIAN_POINT('Origin',(19.,19.,39.9));
#8229=CARTESIAN_POINT('',(18.725,19.,40.));
#8230=CARTESIAN_POINT('Origin',(19.,19.,40.));
#8231=CARTESIAN_POINT('',(18.725,19.,39.9));
#8232=CARTESIAN_POINT('Origin',(20.,20.,40.));
#8233=CARTESIAN_POINT('',(20.,20.,40.));
#8234=CARTESIAN_POINT('',(-20.,20.,40.));
#8235=CARTESIAN_POINT('',(20.,20.,40.));
#8236=CARTESIAN_POINT('',(-20.,20.,41.2));
#8237=CARTESIAN_POINT('',(-20.,20.,40.));
#8238=CARTESIAN_POINT('',(20.,20.,41.2));
#8239=CARTESIAN_POINT('',(20.,20.,41.2));
#8240=CARTESIAN_POINT('',(20.,20.,40.));
#8241=CARTESIAN_POINT('Origin',(20.,-20.,40.));
#8242=CARTESIAN_POINT('',(20.,-20.,40.));
#8243=CARTESIAN_POINT('',(20.,-20.,40.));
#8244=CARTESIAN_POINT('',(20.,-20.,41.2));
#8245=CARTESIAN_POINT('',(20.,-20.,41.2));
#8246=CARTESIAN_POINT('',(20.,-20.,40.));
#8247=CARTESIAN_POINT('Origin',(-20.,-20.,40.));
#8248=CARTESIAN_POINT('',(-20.,-20.,40.));
#8249=CARTESIAN_POINT('',(-20.,-20.,40.));
#8250=CARTESIAN_POINT('',(-20.,-20.,41.2));
#8251=CARTESIAN_POINT('',(-20.,-20.,41.2));
#8252=CARTESIAN_POINT('',(-20.,-20.,40.));
#8253=CARTESIAN_POINT('Origin',(-20.,20.,40.));
#8254=CARTESIAN_POINT('',(-20.,20.,40.));
#8255=CARTESIAN_POINT('',(-20.,20.,41.2));
#8256=CARTESIAN_POINT('Origin',(0.,0.,41.2));
#8257=CARTESIAN_POINT('Origin',(0.,0.,40.));
#8258=CARTESIAN_POINT('',(0.,0.,0.));
#8259=CARTESIAN_POINT('Origin',(19.,-10.,4.9));
#8260=CARTESIAN_POINT('',(18.725,-10.,5.));
#8261=CARTESIAN_POINT('Origin',(19.,-10.,5.));
#8262=CARTESIAN_POINT('',(18.725,-10.,5.8));
#8263=CARTESIAN_POINT('',(18.725,-10.,4.9));
#8264=CARTESIAN_POINT('Origin',(19.,-10.,5.8));
#8265=CARTESIAN_POINT('Origin',(-19.,10.,4.9));
#8266=CARTESIAN_POINT('',(-19.275,10.,5.));
#8267=CARTESIAN_POINT('Origin',(-19.,10.,5.));
#8268=CARTESIAN_POINT('',(-19.275,10.,5.8));
#8269=CARTESIAN_POINT('',(-19.275,10.,4.9));
#8270=CARTESIAN_POINT('Origin',(-19.,10.,5.8));
#8271=CARTESIAN_POINT('Origin',(-19.,-10.,4.9));
#8272=CARTESIAN_POINT('',(-19.275,-10.,5.));
#8273=CARTESIAN_POINT('Origin',(-19.,-10.,5.));
#8274=CARTESIAN_POINT('',(-19.275,-10.,5.8));
#8275=CARTESIAN_POINT('',(-19.275,-10.,4.9));
#8276=CARTESIAN_POINT('Origin',(-19.,-10.,5.8));
#8277=CARTESIAN_POINT('Origin',(19.,10.,4.9));
#8278=CARTESIAN_POINT('',(18.725,10.,5.));
#8279=CARTESIAN_POINT('Origin',(19.,10.,5.));
#8280=CARTESIAN_POINT('',(18.725,10.,5.8));
#8281=CARTESIAN_POINT('',(18.725,10.,4.9));
#8282=CARTESIAN_POINT('Origin',(19.,10.,5.8));
#8283=CARTESIAN_POINT('Origin',(18.,18.,4.9));
#8284=CARTESIAN_POINT('',(18.,18.,5.));
#8285=CARTESIAN_POINT('',(20.,18.,5.));
#8286=CARTESIAN_POINT('',(9.,18.,5.));
#8287=CARTESIAN_POINT('',(18.,18.,5.8));
#8288=CARTESIAN_POINT('',(18.,18.,4.9));
#8289=CARTESIAN_POINT('',(20.,18.,5.8));
#8290=CARTESIAN_POINT('',(9.,18.,5.8));
#8291=CARTESIAN_POINT('',(20.,18.,4.95));
#8292=CARTESIAN_POINT('Origin',(18.,20.,4.9));
#8293=CARTESIAN_POINT('',(18.,20.,5.));
#8294=CARTESIAN_POINT('',(18.,10.,5.));
#8295=CARTESIAN_POINT('',(18.,20.,5.8));
#8296=CARTESIAN_POINT('',(18.,20.,4.95));
#8297=CARTESIAN_POINT('',(18.,10.,5.8));
#8298=CARTESIAN_POINT('Origin',(20.,-20.,5.));
#8299=CARTESIAN_POINT('',(20.,-18.,5.8));
#8300=CARTESIAN_POINT('',(20.,-20.,5.8));
#8301=CARTESIAN_POINT('',(20.,-18.,5.));
#8302=CARTESIAN_POINT('',(20.,-18.,4.95));
#8303=CARTESIAN_POINT('',(20.,-20.,5.));
#8304=CARTESIAN_POINT('Origin',(0.,0.,5.8));
#8305=CARTESIAN_POINT('',(-18.,20.,5.8));
#8306=CARTESIAN_POINT('',(20.,20.,5.8));
#8307=CARTESIAN_POINT('',(-18.,18.,5.8));
#8308=CARTESIAN_POINT('',(-18.,9.,5.8));
#8309=CARTESIAN_POINT('',(-20.,18.,5.8));
#8310=CARTESIAN_POINT('',(-10.,18.,5.8));
#8311=CARTESIAN_POINT('',(-20.,-18.,5.8));
#8312=CARTESIAN_POINT('',(-20.,20.,5.8));
#8313=CARTESIAN_POINT('',(-18.,-18.,5.8));
#8314=CARTESIAN_POINT('',(-9.,-18.,5.8));
#8315=CARTESIAN_POINT('',(-18.,-20.,5.8));
#8316=CARTESIAN_POINT('',(-18.,-10.,5.8));
#8317=CARTESIAN_POINT('',(18.,-20.,5.8));
#8318=CARTESIAN_POINT('',(-20.,-20.,5.8));
#8319=CARTESIAN_POINT('',(18.,-18.,5.8));
#8320=CARTESIAN_POINT('',(18.,-9.,5.8));
#8321=CARTESIAN_POINT('',(10.,-18.,5.8));
#8322=CARTESIAN_POINT('Origin',(18.,-18.,4.9));
#8323=CARTESIAN_POINT('',(18.,-18.,5.));
#8324=CARTESIAN_POINT('',(18.,-20.,5.));
#8325=CARTESIAN_POINT('',(18.,-9.,5.));
#8326=CARTESIAN_POINT('',(18.,-18.,4.9));
#8327=CARTESIAN_POINT('',(18.,-20.,4.95));
#8328=CARTESIAN_POINT('Origin',(20.,-18.,4.9));
#8329=CARTESIAN_POINT('',(10.,-18.,5.));
#8330=CARTESIAN_POINT('Origin',(-20.,-20.,5.));
#8331=CARTESIAN_POINT('',(-18.,-20.,5.));
#8332=CARTESIAN_POINT('',(-18.,-20.,4.95));
#8333=CARTESIAN_POINT('',(-20.,-20.,5.));
#8334=CARTESIAN_POINT('Origin',(-18.,18.,4.9));
#8335=CARTESIAN_POINT('',(-18.,18.,5.));
#8336=CARTESIAN_POINT('',(-18.,20.,5.));
#8337=CARTESIAN_POINT('',(-18.,9.,5.));
#8338=CARTESIAN_POINT('',(-18.,18.,4.9));
#8339=CARTESIAN_POINT('',(-18.,20.,4.95));
#8340=CARTESIAN_POINT('Origin',(-20.,18.,4.9));
#8341=CARTESIAN_POINT('',(-20.,18.,5.));
#8342=CARTESIAN_POINT('',(-10.,18.,5.));
#8343=CARTESIAN_POINT('',(-20.,18.,4.95));
#8344=CARTESIAN_POINT('Origin',(20.,20.,5.));
#8345=CARTESIAN_POINT('',(20.,20.,5.));
#8346=CARTESIAN_POINT('Origin',(-18.,-20.,4.9));
#8347=CARTESIAN_POINT('',(-18.,-18.,5.));
#8348=CARTESIAN_POINT('',(-18.,-18.,4.9));
#8349=CARTESIAN_POINT('',(-18.,-10.,5.));
#8350=CARTESIAN_POINT('Origin',(-18.,-18.,4.9));
#8351=CARTESIAN_POINT('',(-20.,-18.,5.));
#8352=CARTESIAN_POINT('',(-20.,-18.,4.95));
#8353=CARTESIAN_POINT('',(-9.,-18.,5.));
#8354=CARTESIAN_POINT('Origin',(-20.,20.,5.));
#8355=CARTESIAN_POINT('',(-20.,20.,5.));
#8356=CARTESIAN_POINT('Origin',(0.,0.,5.));
#8357=CARTESIAN_POINT('',(0.,0.,0.));
#8358=CARTESIAN_POINT('Origin',(-10.,22.5,38.9));
#8359=CARTESIAN_POINT('',(-10.165,22.5,39.));
#8360=CARTESIAN_POINT('Origin',(-10.,22.5,39.));
#8361=CARTESIAN_POINT('',(-10.165,22.5,39.8));
#8362=CARTESIAN_POINT('',(-10.165,22.5,38.9));
#8363=CARTESIAN_POINT('Origin',(-10.,22.5,39.8));
#8364=CARTESIAN_POINT('Origin',(-10.8,19.9,37.));
#8365=CARTESIAN_POINT('',(-11.075,20.,37.));
#8366=CARTESIAN_POINT('Origin',(-10.8,20.,37.));
#8367=CARTESIAN_POINT('',(-11.075,20.8,37.));
#8368=CARTESIAN_POINT('',(-11.075,19.9,37.));
#8369=CARTESIAN_POINT('Origin',(-10.8,20.8,37.));
#8370=CARTESIAN_POINT('Origin',(-9.2,19.9,37.));
#8371=CARTESIAN_POINT('',(-9.475,20.,37.));
#8372=CARTESIAN_POINT('Origin',(-9.2,20.,37.));
#8373=CARTESIAN_POINT('',(-9.475,20.8,37.));
#8374=CARTESIAN_POINT('',(-9.475,19.9,37.));
#8375=CARTESIAN_POINT('Origin',(-9.2,20.8,37.));
#8376=CARTESIAN_POINT('Origin',(-12.,23.,39.8));
#8377=CARTESIAN_POINT('',(-12.,23.,39.8));
#8378=CARTESIAN_POINT('',(-12.,20.,39.8));
#8379=CARTESIAN_POINT('',(-12.,23.,39.8));
#8380=CARTESIAN_POINT('',(-8.,20.,39.8));
#8381=CARTESIAN_POINT('',(-12.,20.,39.8));
#8382=CARTESIAN_POINT('',(-8.,23.,39.8));
#8383=CARTESIAN_POINT('',(-8.,23.,39.8));
#8384=CARTESIAN_POINT('',(-12.,23.,39.8));
#8385=CARTESIAN_POINT('Origin',(-12.,23.,39.));
#8386=CARTESIAN_POINT('',(-12.,23.,39.));
#8387=CARTESIAN_POINT('',(-12.,23.,39.));
#8388=CARTESIAN_POINT('',(-8.,23.,39.));
#8389=CARTESIAN_POINT('',(-8.,23.,39.));
#8390=CARTESIAN_POINT('',(-12.,23.,39.));
#8391=CARTESIAN_POINT('Origin',(-12.,20.8,39.));
#8392=CARTESIAN_POINT('',(-12.,20.8,39.));
#8393=CARTESIAN_POINT('',(-12.,20.8,39.));
#8394=CARTESIAN_POINT('',(-8.,20.8,39.));
#8395=CARTESIAN_POINT('',(-8.,20.8,39.));
#8396=CARTESIAN_POINT('',(-12.,20.8,39.));
#8397=CARTESIAN_POINT('Origin',(-12.,20.8,35.));
#8398=CARTESIAN_POINT('',(-12.,20.8,35.));
#8399=CARTESIAN_POINT('',(-12.,20.8,35.));
#8400=CARTESIAN_POINT('',(-8.,20.8,35.));
#8401=CARTESIAN_POINT('',(-8.,20.8,35.));
#8402=CARTESIAN_POINT('',(-12.,20.8,35.));
#8403=CARTESIAN_POINT('Origin',(-12.,20.,35.));
#8404=CARTESIAN_POINT('',(-12.,20.,35.));
#8405=CARTESIAN_POINT('',(-12.,20.,35.));
#8406=CARTESIAN_POINT('',(-8.,20.,35.));
#8407=CARTESIAN_POINT('',(-8.,20.,35.));
#8408=CARTESIAN_POINT('',(-12.,20.,35.));
#8409=CARTESIAN_POINT('Origin',(-12.,20.,39.8));
#8410=CARTESIAN_POINT('',(-12.,20.,39.8));
#8411=CARTESIAN_POINT('',(-8.,20.,39.8));
#8412=CARTESIAN_POINT('Origin',(-8.,21.5,37.4));
#8413=CARTESIAN_POINT('Origin',(-12.,21.5,37.4));
#8414=CARTESIAN_POINT('',(0.,0.,0.));
#8415=CARTESIAN_POINT('Origin',(10.,22.5,38.9));
#8416=CARTESIAN_POINT('',(9.835,22.5,39.));
#8417=CARTESIAN_POINT('Origin',(10.,22.5,39.));
#8418=CARTESIAN_POINT('',(9.835,22.5,39.8));
#8419=CARTESIAN_POINT('',(9.835,22.5,38.9));
#8420=CARTESIAN_POINT('Origin',(10.,22.5,39.8));
#8421=CARTESIAN_POINT('Origin',(9.2,19.9,37.));
#8422=CARTESIAN_POINT('',(8.925,20.,37.));
#8423=CARTESIAN_POINT('Origin',(9.2,20.,37.));
#8424=CARTESIAN_POINT('',(8.925,20.8,37.));
#8425=CARTESIAN_POINT('',(8.925,19.9,37.));
#8426=CARTESIAN_POINT('Origin',(9.2,20.8,37.));
#8427=CARTESIAN_POINT('Origin',(10.8,19.9,37.));
#8428=CARTESIAN_POINT('',(10.525,20.,37.));
#8429=CARTESIAN_POINT('Origin',(10.8,20.,37.));
#8430=CARTESIAN_POINT('',(10.525,20.8,37.));
#8431=CARTESIAN_POINT('',(10.525,19.9,37.));
#8432=CARTESIAN_POINT('Origin',(10.8,20.8,37.));
#8433=CARTESIAN_POINT('Origin',(8.,23.,39.8));
#8434=CARTESIAN_POINT('',(8.,23.,39.8));
#8435=CARTESIAN_POINT('',(8.,20.,39.8));
#8436=CARTESIAN_POINT('',(8.,23.,39.8));
#8437=CARTESIAN_POINT('',(12.,20.,39.8));
#8438=CARTESIAN_POINT('',(8.,20.,39.8));
#8439=CARTESIAN_POINT('',(12.,23.,39.8));
#8440=CARTESIAN_POINT('',(12.,23.,39.8));
#8441=CARTESIAN_POINT('',(8.,23.,39.8));
#8442=CARTESIAN_POINT('Origin',(8.,23.,39.));
#8443=CARTESIAN_POINT('',(8.,23.,39.));
#8444=CARTESIAN_POINT('',(8.,23.,39.));
#8445=CARTESIAN_POINT('',(12.,23.,39.));
#8446=CARTESIAN_POINT('',(12.,23.,39.));
#8447=CARTESIAN_POINT('',(8.,23.,39.));
#8448=CARTESIAN_POINT('Origin',(8.,20.8,39.));
#8449=CARTESIAN_POINT('',(8.,20.8,39.));
#8450=CARTESIAN_POINT('',(8.,20.8,39.));
#8451=CARTESIAN_POINT('',(12.,20.8,39.));
#8452=CARTESIAN_POINT('',(12.,20.8,39.));
#8453=CARTESIAN_POINT('',(8.,20.8,39.));
#8454=CARTESIAN_POINT('Origin',(8.,20.8,35.));
#8455=CARTESIAN_POINT('',(8.,20.8,35.));
#8456=CARTESIAN_POINT('',(8.,20.8,35.));
#8457=CARTESIAN_POINT('',(12.,20.8,35.));
#8458=CARTESIAN_POINT('',(12.,20.8,35.));
#8459=CARTESIAN_POINT('',(8.,20.8,35.));
#8460=CARTESIAN_POINT('Origin',(8.,20.,35.));
#8461=CARTESIAN_POINT('',(8.,20.,35.));
#8462=CARTESIAN_POINT('',(8.,20.,35.));
#8463=CARTESIAN_POINT('',(12.,20.,35.));
#8464=CARTESIAN_POINT('',(12.,20.,35.));
#8465=CARTESIAN_POINT('',(8.,20.,35.));
#8466=CARTESIAN_POINT('Origin',(8.,20.,39.8));
#8467=CARTESIAN_POINT('',(8.,20.,39.8));
#8468=CARTESIAN_POINT('',(12.,20.,39.8));
#8469=CARTESIAN_POINT('Origin',(12.,21.5,37.4));
#8470=CARTESIAN_POINT('Origin',(8.,21.5,37.4));
#8471=CARTESIAN_POINT('',(0.,0.,0.));
#8472=CARTESIAN_POINT('Origin',(-10.,22.5,39.7));
#8473=CARTESIAN_POINT('',(-10.225,22.5,39.8));
#8474=CARTESIAN_POINT('Origin',(-10.,22.5,39.8));
#8475=CARTESIAN_POINT('',(-10.225,22.5,40.6));
#8476=CARTESIAN_POINT('',(-10.225,22.5,39.7));
#8477=CARTESIAN_POINT('Origin',(-10.,22.5,40.6));
#8478=CARTESIAN_POINT('Origin',(10.,22.5,39.7));
#8479=CARTESIAN_POINT('',(9.775,22.5,39.8));
#8480=CARTESIAN_POINT('Origin',(10.,22.5,39.8));
#8481=CARTESIAN_POINT('',(9.775,22.5,40.6));
#8482=CARTESIAN_POINT('',(9.775,22.5,39.7));
#8483=CARTESIAN_POINT('Origin',(10.,22.5,40.6));
#8484=CARTESIAN_POINT('Origin',(14.,23.,39.8));
#8485=CARTESIAN_POINT('',(14.,23.,39.8));
#8486=CARTESIAN_POINT('',(-14.,23.,39.8));
#8487=CARTESIAN_POINT('',(14.,23.,39.8));
#8488=CARTESIAN_POINT('',(-14.,23.,40.6));
#8489=CARTESIAN_POINT('',(-14.,23.,39.8));
#8490=CARTESIAN_POINT('',(14.,23.,40.6));
#8491=CARTESIAN_POINT('',(14.,23.,40.6));
#8492=CARTESIAN_POINT('',(14.,23.,39.8));
#8493=CARTESIAN_POINT('Origin',(14.,22.,39.8));
#8494=CARTESIAN_POINT('',(14.,22.,39.8));
#8495=CARTESIAN_POINT('',(14.,22.,39.8));
#8496=CARTESIAN_POINT('',(14.,22.,40.6));
#8497=CARTESIAN_POINT('',(14.,22.,40.6));
#8498=CARTESIAN_POINT('',(14.,22.,39.8));
#8499=CARTESIAN_POINT('Origin',(-14.,22.,39.8));
#8500=CARTESIAN_POINT('',(-14.,22.,39.8));
#8501=CARTESIAN_POINT('',(-14.,22.,39.8));
#8502=CARTESIAN_POINT('',(-14.,22.,40.6));
#8503=CARTESIAN_POINT('',(-14.,22.,40.6));
#8504=CARTESIAN_POINT('',(-14.,22.,39.8));
#8505=CARTESIAN_POINT('Origin',(-14.,23.,39.8));
#8506=CARTESIAN_POINT('',(-14.,23.,39.8));
#8507=CARTESIAN_POINT('',(-14.,23.,40.6));
#8508=CARTESIAN_POINT('Origin',(0.,22.5,40.6));
#8509=CARTESIAN_POINT('Origin',(0.,22.5,39.8));
#8510=CARTESIAN_POINT('',(0.,0.,0.));
#8511=CARTESIAN_POINT('Origin',(4.,-1.1,0.));
#8512=CARTESIAN_POINT('',(3.725,-0.42,3.36777869765523E-17));
#8513=CARTESIAN_POINT('Origin',(4.,-0.42,0.));
#8514=CARTESIAN_POINT('',(3.725,-0.21,6.36764273396499E-17));
#8515=CARTESIAN_POINT('',(3.725,-1.1,3.36777869765523E-17));
#8516=CARTESIAN_POINT('',(3.82244719095435,-2.57175827820944E-17,0.21));
#8517=CARTESIAN_POINT('Ctrl Pts',(3.82244719095435,-3.81639164714898E-17,
0.21));
#8518=CARTESIAN_POINT('Ctrl Pts',(3.82244719095435,-0.0141630178371274,
0.21));
#8519=CARTESIAN_POINT('Ctrl Pts',(3.82070090566933,-0.0283388251429181,
0.208554382393535));
#8520=CARTESIAN_POINT('Ctrl Pts',(3.81433611385284,-0.0559106681449084,
0.202908887997328));
#8521=CARTESIAN_POINT('Ctrl Pts',(3.80974723471181,-0.0693141634661026,
0.198712082533353));
#8522=CARTESIAN_POINT('Ctrl Pts',(3.7937414503193,-0.107475484252795,0.182517999394844));
#8523=CARTESIAN_POINT('Ctrl Pts',(3.78023922617715,-0.130251970586776,0.166732877511574));
#8524=CARTESIAN_POINT('Ctrl Pts',(3.75710894103549,-0.166306329654162,0.130678518444188));
#8525=CARTESIAN_POINT('Ctrl Pts',(3.74560158587233,-0.182341144032027,0.107860332287474));
#8526=CARTESIAN_POINT('Ctrl Pts',(3.72949374752356,-0.204214038345313,0.0563806217319966));
#8527=CARTESIAN_POINT('Ctrl Pts',(3.725,-0.21,0.0276636393226111));
#8528=CARTESIAN_POINT('Ctrl Pts',(3.725,-0.21,0.));
#8529=CARTESIAN_POINT('',(3.725,0.21,9.8999995843689E-18));
#8530=CARTESIAN_POINT('Ctrl Pts',(3.725,0.21,-1.04083408558608E-17));
#8531=CARTESIAN_POINT('Ctrl Pts',(3.725,0.21,0.027663639322611));
#8532=CARTESIAN_POINT('Ctrl Pts',(3.72949374752356,0.204214038345313,0.0563806217319965));
#8533=CARTESIAN_POINT('Ctrl Pts',(3.74560158587233,0.182341144032027,0.107860332287474));
#8534=CARTESIAN_POINT('Ctrl Pts',(3.75710894103549,0.166306329654162,0.130678518444188));
#8535=CARTESIAN_POINT('Ctrl Pts',(3.78023922617715,0.130251970586776,0.166732877511574));
#8536=CARTESIAN_POINT('Ctrl Pts',(3.7937414503193,0.107475484252795,0.182517999394844));
#8537=CARTESIAN_POINT('Ctrl Pts',(3.80974723471181,0.0693141634661026,0.198712082533353));
#8538=CARTESIAN_POINT('Ctrl Pts',(3.81433611385284,0.0559106681449085,0.202908887997328));
#8539=CARTESIAN_POINT('Ctrl Pts',(3.82070090566933,0.0283388251429181,0.208554382393535));
#8540=CARTESIAN_POINT('Ctrl Pts',(3.82244719095435,0.0141630178371274,0.21));
#8541=CARTESIAN_POINT('Ctrl Pts',(3.82244719095435,3.46944695195361E-17,
0.21));
#8542=CARTESIAN_POINT('',(3.725,0.42,-3.36777869765523E-17));
#8543=CARTESIAN_POINT('',(3.725,-1.1,3.36777869765523E-17));
#8544=CARTESIAN_POINT('Origin',(4.,0.42,0.));
#8545=CARTESIAN_POINT('',(3.82244719095435,-3.46944695195361E-18,-0.21));
#8546=CARTESIAN_POINT('Ctrl Pts',(3.82244719095435,-3.46944695195361E-18,
-0.21));
#8547=CARTESIAN_POINT('Ctrl Pts',(3.82244719095435,0.0141630178371273,-0.21));
#8548=CARTESIAN_POINT('Ctrl Pts',(3.82070090566933,0.028338825142918,-0.208554382393535));
#8549=CARTESIAN_POINT('Ctrl Pts',(3.81433611385284,0.0559106681449083,-0.202908887997328));
#8550=CARTESIAN_POINT('Ctrl Pts',(3.80974723471181,0.0693141634661026,-0.198712082533353));
#8551=CARTESIAN_POINT('Ctrl Pts',(3.7937414503193,0.107475484252795,-0.182517999394844));
#8552=CARTESIAN_POINT('Ctrl Pts',(3.78023922617715,0.130251970586776,-0.166732877511574));
#8553=CARTESIAN_POINT('Ctrl Pts',(3.75710894103549,0.166306329654162,-0.130678518444188));
#8554=CARTESIAN_POINT('Ctrl Pts',(3.74560158587233,0.182341144032027,-0.107860332287474));
#8555=CARTESIAN_POINT('Ctrl Pts',(3.72949374752356,0.204214038345313,-0.0563806217319966));
#8556=CARTESIAN_POINT('Ctrl Pts',(3.725,0.21,-0.027663639322611));
#8557=CARTESIAN_POINT('Ctrl Pts',(3.725,0.21,2.77555756156289E-17));
#8558=CARTESIAN_POINT('Ctrl Pts',(3.725,-0.21,9.36750677027476E-17));
#8559=CARTESIAN_POINT('Ctrl Pts',(3.725,-0.21,-0.027663639322611));
#8560=CARTESIAN_POINT('Ctrl Pts',(3.72949374752356,-0.204214038345313,-0.0563806217319965));
#8561=CARTESIAN_POINT('Ctrl Pts',(3.74560158587233,-0.182341144032027,-0.107860332287474));
#8562=CARTESIAN_POINT('Ctrl Pts',(3.75710894103549,-0.166306329654162,-0.130678518444188));
#8563=CARTESIAN_POINT('Ctrl Pts',(3.78023922617715,-0.130251970586776,-0.166732877511574));
#8564=CARTESIAN_POINT('Ctrl Pts',(3.7937414503193,-0.107475484252795,-0.182517999394844));
#8565=CARTESIAN_POINT('Ctrl Pts',(3.80974723471181,-0.0693141634661024,
-0.198712082533353));
#8566=CARTESIAN_POINT('Ctrl Pts',(3.81433611385284,-0.0559106681449084,
-0.202908887997328));
#8567=CARTESIAN_POINT('Ctrl Pts',(3.82070090566933,-0.0283388251429182,
-0.208554382393535));
#8568=CARTESIAN_POINT('Ctrl Pts',(3.82244719095435,-0.0141630178371273,
-0.21));
#8569=CARTESIAN_POINT('Ctrl Pts',(3.82244719095435,-3.46944695195361E-18,
-0.21));
#8570=CARTESIAN_POINT('',(4.17755280904565,-3.12250225675825E-17,-0.21));
#8571=CARTESIAN_POINT('',(4.17755280904565,-2.57175827820944E-17,0.21));
#8572=CARTESIAN_POINT('Ctrl Pts',(4.17755280904565,-3.12250225675825E-17,
-0.21));
#8573=CARTESIAN_POINT('Ctrl Pts',(4.17755280904565,-0.0141630178371274,
-0.21));
#8574=CARTESIAN_POINT('Ctrl Pts',(4.17929909433067,-0.0283388251429182,
-0.208554382393535));
#8575=CARTESIAN_POINT('Ctrl Pts',(4.18566388614715,-0.0559106681449083,
-0.202908887997328));
#8576=CARTESIAN_POINT('Ctrl Pts',(4.19025276528819,-0.0693141634661022,
-0.198712082533353));
#8577=CARTESIAN_POINT('Ctrl Pts',(4.2062585496807,-0.107475484252795,-0.182517999394844));
#8578=CARTESIAN_POINT('Ctrl Pts',(4.21976077382285,-0.130251970586776,-0.166732877511574));
#8579=CARTESIAN_POINT('Ctrl Pts',(4.24289105896451,-0.166306329654162,-0.130678518444188));
#8580=CARTESIAN_POINT('Ctrl Pts',(4.25439841412767,-0.182341144032028,-0.107860332287473));
#8581=CARTESIAN_POINT('Ctrl Pts',(4.27050625247645,-0.204214038345313,-0.0563806217319961));
#8582=CARTESIAN_POINT('Ctrl Pts',(4.275,-0.21,-0.027663639322611));
#8583=CARTESIAN_POINT('Ctrl Pts',(4.275,-0.21,0.0276636393226111));
#8584=CARTESIAN_POINT('Ctrl Pts',(4.27050625247645,-0.204214038345313,0.0563806217319962));
#8585=CARTESIAN_POINT('Ctrl Pts',(4.25439841412767,-0.182341144032028,0.107860332287473));
#8586=CARTESIAN_POINT('Ctrl Pts',(4.24289105896451,-0.166306329654162,0.130678518444188));
#8587=CARTESIAN_POINT('Ctrl Pts',(4.21976077382285,-0.130251970586776,0.166732877511574));
#8588=CARTESIAN_POINT('Ctrl Pts',(4.2062585496807,-0.107475484252794,0.182517999394844));
#8589=CARTESIAN_POINT('Ctrl Pts',(4.19025276528819,-0.0693141634661021,
0.198712082533353));
#8590=CARTESIAN_POINT('Ctrl Pts',(4.18566388614715,-0.0559106681449083,
0.202908887997328));
#8591=CARTESIAN_POINT('Ctrl Pts',(4.17929909433067,-0.0283388251429182,
0.208554382393535));
#8592=CARTESIAN_POINT('Ctrl Pts',(4.17755280904565,-0.0141630178371274,
0.21));
#8593=CARTESIAN_POINT('Ctrl Pts',(4.17755280904565,-1.04083408558608E-17,
0.21));
#8594=CARTESIAN_POINT('Ctrl Pts',(4.17755280904565,1.38777878078145E-17,
0.21));
#8595=CARTESIAN_POINT('Ctrl Pts',(4.17755280904565,0.0141630178371274,0.21));
#8596=CARTESIAN_POINT('Ctrl Pts',(4.17929909433067,0.0283388251429182,0.208554382393535));
#8597=CARTESIAN_POINT('Ctrl Pts',(4.18566388614715,0.0559106681449083,0.202908887997328));
#8598=CARTESIAN_POINT('Ctrl Pts',(4.19025276528819,0.0693141634661021,0.198712082533353));
#8599=CARTESIAN_POINT('Ctrl Pts',(4.2062585496807,0.107475484252794,0.182517999394844));
#8600=CARTESIAN_POINT('Ctrl Pts',(4.21976077382285,0.130251970586776,0.166732877511574));
#8601=CARTESIAN_POINT('Ctrl Pts',(4.24289105896451,0.166306329654162,0.130678518444188));
#8602=CARTESIAN_POINT('Ctrl Pts',(4.25439841412767,0.182341144032028,0.107860332287473));
#8603=CARTESIAN_POINT('Ctrl Pts',(4.27050625247645,0.204214038345313,0.0563806217319961));
#8604=CARTESIAN_POINT('Ctrl Pts',(4.275,0.21,0.027663639322611));
#8605=CARTESIAN_POINT('Ctrl Pts',(4.275,0.21,-0.027663639322611));
#8606=CARTESIAN_POINT('Ctrl Pts',(4.27050625247645,0.204214038345313,-0.0563806217319961));
#8607=CARTESIAN_POINT('Ctrl Pts',(4.25439841412767,0.182341144032028,-0.107860332287473));
#8608=CARTESIAN_POINT('Ctrl Pts',(4.24289105896451,0.166306329654162,-0.130678518444188));
#8609=CARTESIAN_POINT('Ctrl Pts',(4.21976077382285,0.130251970586776,-0.166732877511574));
#8610=CARTESIAN_POINT('Ctrl Pts',(4.2062585496807,0.107475484252794,-0.182517999394844));
#8611=CARTESIAN_POINT('Ctrl Pts',(4.19025276528819,0.0693141634661021,-0.198712082533353));
#8612=CARTESIAN_POINT('Ctrl Pts',(4.18566388614715,0.0559106681449083,-0.202908887997328));
#8613=CARTESIAN_POINT('Ctrl Pts',(4.17929909433067,0.0283388251429182,-0.208554382393535));
#8614=CARTESIAN_POINT('Ctrl Pts',(4.17755280904565,0.0141630178371273,-0.21));
#8615=CARTESIAN_POINT('Ctrl Pts',(4.17755280904565,0.,-0.21));
#8616=CARTESIAN_POINT('Origin',(34.,-1.1,0.));
#8617=CARTESIAN_POINT('',(33.725,-0.42,3.3677786976552E-17));
#8618=CARTESIAN_POINT('Origin',(34.,-0.42,0.));
#8619=CARTESIAN_POINT('',(33.725,-0.21,4.28597456279281E-17));
#8620=CARTESIAN_POINT('',(33.725,-1.1,3.3677786976552E-17));
#8621=CARTESIAN_POINT('',(33.8224471909544,-2.57175827820944E-17,0.21));
#8622=CARTESIAN_POINT('Ctrl Pts',(33.8224471909543,-3.40005801291454E-16,
0.21));
#8623=CARTESIAN_POINT('Ctrl Pts',(33.8224471909543,-0.0141630178371276,
0.21));
#8624=CARTESIAN_POINT('Ctrl Pts',(33.8207009056693,-0.0283388251429169,
0.208554382393535));
#8625=CARTESIAN_POINT('Ctrl Pts',(33.8143361138529,-0.0559106681449082,
0.202908887997328));
#8626=CARTESIAN_POINT('Ctrl Pts',(33.8097472347118,-0.0693141634661021,
0.198712082533353));
#8627=CARTESIAN_POINT('Ctrl Pts',(33.7937414503193,-0.107475484252794,0.182517999394844));
#8628=CARTESIAN_POINT('Ctrl Pts',(33.7802392261772,-0.130251970586776,0.166732877511574));
#8629=CARTESIAN_POINT('Ctrl Pts',(33.7571089410355,-0.166306329654162,0.130678518444188));
#8630=CARTESIAN_POINT('Ctrl Pts',(33.7456015858723,-0.182341144032027,0.107860332287474));
#8631=CARTESIAN_POINT('Ctrl Pts',(33.7294937475236,-0.204214038345313,0.0563806217319973));
#8632=CARTESIAN_POINT('Ctrl Pts',(33.725,-0.21,0.027663639322611));
#8633=CARTESIAN_POINT('Ctrl Pts',(33.725,-0.21,-2.63677968348475E-16));
#8634=CARTESIAN_POINT('',(33.725,0.21,6.02069803876962E-17));
#8635=CARTESIAN_POINT('Ctrl Pts',(33.725,0.21,9.0205620750794E-17));
#8636=CARTESIAN_POINT('Ctrl Pts',(33.725,0.21,0.0276636393226113));
#8637=CARTESIAN_POINT('Ctrl Pts',(33.7294937475236,0.204214038345313,0.0563806217319973));
#8638=CARTESIAN_POINT('Ctrl Pts',(33.7456015858723,0.182341144032027,0.107860332287474));
#8639=CARTESIAN_POINT('Ctrl Pts',(33.7571089410355,0.166306329654162,0.130678518444188));
#8640=CARTESIAN_POINT('Ctrl Pts',(33.7802392261772,0.130251970586776,0.166732877511574));
#8641=CARTESIAN_POINT('Ctrl Pts',(33.7937414503193,0.107475484252794,0.182517999394844));
#8642=CARTESIAN_POINT('Ctrl Pts',(33.8097472347118,0.0693141634661021,0.198712082533353));
#8643=CARTESIAN_POINT('Ctrl Pts',(33.8143361138529,0.0559106681449082,0.202908887997328));
#8644=CARTESIAN_POINT('Ctrl Pts',(33.8207009056693,0.0283388251429169,0.208554382393535));
#8645=CARTESIAN_POINT('Ctrl Pts',(33.8224471909543,0.0141630178371276,0.21));
#8646=CARTESIAN_POINT('Ctrl Pts',(33.8224471909543,3.36536354339501E-16,
0.21));
#8647=CARTESIAN_POINT('',(33.725,0.42,-3.3677786976552E-17));
#8648=CARTESIAN_POINT('',(33.725,-1.1,3.3677786976552E-17));
#8649=CARTESIAN_POINT('Origin',(34.,0.42,0.));
#8650=CARTESIAN_POINT('',(33.8224471909543,2.67147415300428E-16,-0.21));
#8651=CARTESIAN_POINT('Ctrl Pts',(33.8224471909543,2.67147415300428E-16,
-0.21));
#8652=CARTESIAN_POINT('Ctrl Pts',(33.8224471909543,0.0141630178371276,-0.21));
#8653=CARTESIAN_POINT('Ctrl Pts',(33.8207009056693,0.028338825142917,-0.208554382393535));
#8654=CARTESIAN_POINT('Ctrl Pts',(33.8143361138529,0.0559106681449084,-0.202908887997328));
#8655=CARTESIAN_POINT('Ctrl Pts',(33.8097472347118,0.0693141634661022,-0.198712082533353));
#8656=CARTESIAN_POINT('Ctrl Pts',(33.7937414503193,0.107475484252794,-0.182517999394844));
#8657=CARTESIAN_POINT('Ctrl Pts',(33.7802392261772,0.130251970586776,-0.166732877511574));
#8658=CARTESIAN_POINT('Ctrl Pts',(33.7571089410355,0.166306329654162,-0.130678518444188));
#8659=CARTESIAN_POINT('Ctrl Pts',(33.7456015858723,0.182341144032027,-0.107860332287474));
#8660=CARTESIAN_POINT('Ctrl Pts',(33.7294937475236,0.204214038345313,-0.0563806217319973));
#8661=CARTESIAN_POINT('Ctrl Pts',(33.725,0.21,-0.0276636393226112));
#8662=CARTESIAN_POINT('Ctrl Pts',(33.725,0.21,-5.20417042793042E-18));
#8663=CARTESIAN_POINT('Ctrl Pts',(33.725,-0.21,4.5102810375397E-17));
#8664=CARTESIAN_POINT('Ctrl Pts',(33.725,-0.21,-0.0276636393226112));
#8665=CARTESIAN_POINT('Ctrl Pts',(33.7294937475236,-0.204214038345313,-0.0563806217319972));
#8666=CARTESIAN_POINT('Ctrl Pts',(33.7456015858723,-0.182341144032027,-0.107860332287474));
#8667=CARTESIAN_POINT('Ctrl Pts',(33.7571089410355,-0.166306329654162,-0.130678518444188));
#8668=CARTESIAN_POINT('Ctrl Pts',(33.7802392261772,-0.130251970586776,-0.166732877511574));
#8669=CARTESIAN_POINT('Ctrl Pts',(33.7937414503193,-0.107475484252794,-0.182517999394844));
#8670=CARTESIAN_POINT('Ctrl Pts',(33.8097472347118,-0.0693141634661023,
-0.198712082533353));
#8671=CARTESIAN_POINT('Ctrl Pts',(33.8143361138529,-0.0559106681449084,
-0.202908887997328));
#8672=CARTESIAN_POINT('Ctrl Pts',(33.8207009056693,-0.028338825142917,-0.208554382393535));
#8673=CARTESIAN_POINT('Ctrl Pts',(33.8224471909544,-0.0141630178371271,
-0.21));
#8674=CARTESIAN_POINT('Ctrl Pts',(33.8224471909544,2.63677968348475E-16,
-0.21));
#8675=CARTESIAN_POINT('',(34.1775528090457,-1.94289029309402E-16,-0.21));
#8676=CARTESIAN_POINT('',(34.1775528090456,-2.57175827820944E-17,0.21));
#8677=CARTESIAN_POINT('Ctrl Pts',(34.1775528090457,-1.94289029309402E-16,
-0.21));
#8678=CARTESIAN_POINT('Ctrl Pts',(34.1775528090457,-0.0141630178371275,
-0.21));
#8679=CARTESIAN_POINT('Ctrl Pts',(34.1792990943307,-0.028338825142917,-0.208554382393535));
#8680=CARTESIAN_POINT('Ctrl Pts',(34.1856638861471,-0.0559106681449084,
-0.202908887997328));
#8681=CARTESIAN_POINT('Ctrl Pts',(34.1902527652882,-0.0693141634661023,
-0.198712082533353));
#8682=CARTESIAN_POINT('Ctrl Pts',(34.2062585496807,-0.107475484252794,-0.182517999394844));
#8683=CARTESIAN_POINT('Ctrl Pts',(34.2197607738228,-0.130251970586776,-0.166732877511574));
#8684=CARTESIAN_POINT('Ctrl Pts',(34.2428910589645,-0.166306329654162,-0.130678518444188));
#8685=CARTESIAN_POINT('Ctrl Pts',(34.2543984141277,-0.182341144032027,-0.107860332287474));
#8686=CARTESIAN_POINT('Ctrl Pts',(34.2705062524764,-0.204214038345313,-0.0563806217319973));
#8687=CARTESIAN_POINT('Ctrl Pts',(34.275,-0.21,-0.0276636393226112));
#8688=CARTESIAN_POINT('Ctrl Pts',(34.275,-0.21,0.0276636393226113));
#8689=CARTESIAN_POINT('Ctrl Pts',(34.2705062524764,-0.204214038345313,0.0563806217319974));
#8690=CARTESIAN_POINT('Ctrl Pts',(34.2543984141277,-0.182341144032027,0.107860332287474));
#8691=CARTESIAN_POINT('Ctrl Pts',(34.2428910589645,-0.166306329654162,0.130678518444188));
#8692=CARTESIAN_POINT('Ctrl Pts',(34.2197607738228,-0.130251970586776,0.166732877511574));
#8693=CARTESIAN_POINT('Ctrl Pts',(34.2062585496807,-0.107475484252794,0.182517999394844));
#8694=CARTESIAN_POINT('Ctrl Pts',(34.1902527652882,-0.0693141634661023,
0.198712082533353));
#8695=CARTESIAN_POINT('Ctrl Pts',(34.1856638861471,-0.0559106681449084,
0.202908887997328));
#8696=CARTESIAN_POINT('Ctrl Pts',(34.1792990943307,-0.028338825142917,0.208554382393535));
#8697=CARTESIAN_POINT('Ctrl Pts',(34.1775528090457,-0.0141630178371273,
0.21));
#8698=CARTESIAN_POINT('Ctrl Pts',(34.1775528090457,1.04083408558608E-17,
0.21));
#8699=CARTESIAN_POINT('Ctrl Pts',(34.1775528090457,-1.38777878078145E-17,
0.21));
#8700=CARTESIAN_POINT('Ctrl Pts',(34.1775528090457,0.0141630178371273,0.21));
#8701=CARTESIAN_POINT('Ctrl Pts',(34.1792990943307,0.028338825142917,0.208554382393535));
#8702=CARTESIAN_POINT('Ctrl Pts',(34.1856638861471,0.0559106681449084,0.202908887997328));
#8703=CARTESIAN_POINT('Ctrl Pts',(34.1902527652882,0.0693141634661023,0.198712082533353));
#8704=CARTESIAN_POINT('Ctrl Pts',(34.2062585496807,0.107475484252794,0.182517999394844));
#8705=CARTESIAN_POINT('Ctrl Pts',(34.2197607738228,0.130251970586776,0.166732877511574));
#8706=CARTESIAN_POINT('Ctrl Pts',(34.2428910589645,0.166306329654162,0.130678518444188));
#8707=CARTESIAN_POINT('Ctrl Pts',(34.2543984141277,0.182341144032027,0.107860332287474));
#8708=CARTESIAN_POINT('Ctrl Pts',(34.2705062524764,0.204214038345313,0.0563806217319973));
#8709=CARTESIAN_POINT('Ctrl Pts',(34.275,0.21,0.0276636393226112));
#8710=CARTESIAN_POINT('Ctrl Pts',(34.275,0.21,-0.0276636393226112));
#8711=CARTESIAN_POINT('Ctrl Pts',(34.2705062524764,0.204214038345313,-0.0563806217319973));
#8712=CARTESIAN_POINT('Ctrl Pts',(34.2543984141277,0.182341144032027,-0.107860332287474));
#8713=CARTESIAN_POINT('Ctrl Pts',(34.2428910589645,0.166306329654162,-0.130678518444188));
#8714=CARTESIAN_POINT('Ctrl Pts',(34.2197607738228,0.130251970586776,-0.166732877511574));
#8715=CARTESIAN_POINT('Ctrl Pts',(34.2062585496807,0.107475484252794,-0.182517999394844));
#8716=CARTESIAN_POINT('Ctrl Pts',(34.1902527652882,0.0693141634661022,-0.198712082533353));
#8717=CARTESIAN_POINT('Ctrl Pts',(34.1856638861471,0.0559106681449084,-0.202908887997328));
#8718=CARTESIAN_POINT('Ctrl Pts',(34.1792990943307,0.028338825142917,-0.208554382393535));
#8719=CARTESIAN_POINT('Ctrl Pts',(34.1775528090456,0.0141630178371274,-0.21));
#8720=CARTESIAN_POINT('Ctrl Pts',(34.1775528090456,1.00613961606655E-16,
-0.21));
#8721=CARTESIAN_POINT('Origin',(-0.1,0.,0.));
#8722=CARTESIAN_POINT('',(-0.1,-2.57175827820944E-17,0.21));
#8723=CARTESIAN_POINT('Origin',(-0.1,0.,0.));
#8724=CARTESIAN_POINT('',(1.17755280904565,0.21,-3.46944695195361E-18));
#8725=CARTESIAN_POINT('',(1.275,-2.45045053518637E-18,0.21));
#8726=CARTESIAN_POINT('Ctrl Pts',(1.17755280904565,0.21,-3.46944695195361E-18));
#8727=CARTESIAN_POINT('Ctrl Pts',(1.17755280904565,0.21,-0.0141630178371274));
#8728=CARTESIAN_POINT('Ctrl Pts',(1.17929909433067,0.208554382393535,-0.0283388251429181));
#8729=CARTESIAN_POINT('Ctrl Pts',(1.18566388614715,0.202908887997328,-0.0559106681449085));
#8730=CARTESIAN_POINT('Ctrl Pts',(1.19025276528819,0.198712082533353,-0.0693141634661026));
#8731=CARTESIAN_POINT('Ctrl Pts',(1.2062585496807,0.182517999394844,-0.107475484252795));
#8732=CARTESIAN_POINT('Ctrl Pts',(1.21976077382285,0.166732877511574,-0.130251970586776));
#8733=CARTESIAN_POINT('Ctrl Pts',(1.24289105896451,0.130678518444188,-0.166306329654162));
#8734=CARTESIAN_POINT('Ctrl Pts',(1.25439841412767,0.107860332287473,-0.182341144032028));
#8735=CARTESIAN_POINT('Ctrl Pts',(1.27050625247644,0.0563806217319963,-0.204214038345313));
#8736=CARTESIAN_POINT('Ctrl Pts',(1.275,0.027663639322611,-0.21));
#8737=CARTESIAN_POINT('Ctrl Pts',(1.275,-0.0276636393226111,-0.21));
#8738=CARTESIAN_POINT('Ctrl Pts',(1.27050625247644,-0.0563806217319964,
-0.204214038345313));
#8739=CARTESIAN_POINT('Ctrl Pts',(1.25439841412767,-0.107860332287474,-0.182341144032027));
#8740=CARTESIAN_POINT('Ctrl Pts',(1.24289105896451,-0.130678518444188,-0.166306329654162));
#8741=CARTESIAN_POINT('Ctrl Pts',(1.21976077382284,-0.166732877511574,-0.130251970586776));
#8742=CARTESIAN_POINT('Ctrl Pts',(1.2062585496807,-0.182517999394844,-0.107475484252795));
#8743=CARTESIAN_POINT('Ctrl Pts',(1.19025276528819,-0.198712082533353,-0.0693141634661024));
#8744=CARTESIAN_POINT('Ctrl Pts',(1.18566388614715,-0.202908887997328,-0.0559106681449083));
#8745=CARTESIAN_POINT('Ctrl Pts',(1.17929909433067,-0.208554382393535,-0.0283388251429181));
#8746=CARTESIAN_POINT('Ctrl Pts',(1.17755280904565,-0.21,-0.0141630178371274));
#8747=CARTESIAN_POINT('Ctrl Pts',(1.17755280904565,-0.21,0.0141630178371274));
#8748=CARTESIAN_POINT('Ctrl Pts',(1.17929909433067,-0.208554382393535,0.0283388251429181));
#8749=CARTESIAN_POINT('Ctrl Pts',(1.18566388614715,-0.202908887997328,0.0559106681449083));
#8750=CARTESIAN_POINT('Ctrl Pts',(1.19025276528819,-0.198712082533353,0.0693141634661024));
#8751=CARTESIAN_POINT('Ctrl Pts',(1.2062585496807,-0.182517999394844,0.107475484252795));
#8752=CARTESIAN_POINT('Ctrl Pts',(1.21976077382284,-0.166732877511574,0.130251970586776));
#8753=CARTESIAN_POINT('Ctrl Pts',(1.24289105896451,-0.130678518444188,0.166306329654162));
#8754=CARTESIAN_POINT('Ctrl Pts',(1.25439841412767,-0.107860332287473,0.182341144032027));
#8755=CARTESIAN_POINT('Ctrl Pts',(1.27050625247644,-0.0563806217319963,
0.204214038345313));
#8756=CARTESIAN_POINT('Ctrl Pts',(1.275,-0.027663639322611,0.21));
#8757=CARTESIAN_POINT('Ctrl Pts',(1.275,4.16333634234434E-17,0.21));
#8758=CARTESIAN_POINT('',(-0.1,-2.57175827820944E-17,0.21));
#8759=CARTESIAN_POINT('Ctrl Pts',(1.275,2.77555756156289E-17,0.21));
#8760=CARTESIAN_POINT('Ctrl Pts',(1.275,0.0276636393226111,0.21));
#8761=CARTESIAN_POINT('Ctrl Pts',(1.27050625247644,0.0563806217319964,0.204214038345313));
#8762=CARTESIAN_POINT('Ctrl Pts',(1.25439841412767,0.107860332287474,0.182341144032027));
#8763=CARTESIAN_POINT('Ctrl Pts',(1.24289105896451,0.130678518444188,0.166306329654162));
#8764=CARTESIAN_POINT('Ctrl Pts',(1.21976077382284,0.166732877511574,0.130251970586776));
#8765=CARTESIAN_POINT('Ctrl Pts',(1.2062585496807,0.182517999394844,0.107475484252795));
#8766=CARTESIAN_POINT('Ctrl Pts',(1.19025276528819,0.198712082533353,0.0693141634661023));
#8767=CARTESIAN_POINT('Ctrl Pts',(1.18566388614715,0.202908887997328,0.0559106681449083));
#8768=CARTESIAN_POINT('Ctrl Pts',(1.17929909433067,0.208554382393535,0.0283388251429181));
#8769=CARTESIAN_POINT('Ctrl Pts',(1.17755280904565,0.21,0.0141630178371273));
#8770=CARTESIAN_POINT('Ctrl Pts',(1.17755280904565,0.21,-1.38777878078145E-17));
#8771=CARTESIAN_POINT('Origin',(1.,0.,-1.1));
#8772=CARTESIAN_POINT('',(0.725,-3.36777869765522E-17,-0.42));
#8773=CARTESIAN_POINT('Origin',(1.,0.,-0.42));
#8774=CARTESIAN_POINT('',(0.725,-3.76555751999978E-17,-0.21));
#8775=CARTESIAN_POINT('',(0.725,-3.36777869765522E-17,-1.1));
#8776=CARTESIAN_POINT('',(0.725,-6.43055263241525E-18,0.21));
#8777=CARTESIAN_POINT('Ctrl Pts',(0.725,2.08166817117217E-17,0.21));
#8778=CARTESIAN_POINT('Ctrl Pts',(0.725,-0.027663639322611,0.21));
#8779=CARTESIAN_POINT('Ctrl Pts',(0.729493747523555,-0.0563806217319963,
0.204214038345313));
#8780=CARTESIAN_POINT('Ctrl Pts',(0.74560158587233,-0.107860332287473,0.182341144032027));
#8781=CARTESIAN_POINT('Ctrl Pts',(0.757108941035492,-0.130678518444188,
0.166306329654162));
#8782=CARTESIAN_POINT('Ctrl Pts',(0.780239226177155,-0.166732877511574,
0.130251970586776));
#8783=CARTESIAN_POINT('Ctrl Pts',(0.793741450319299,-0.182517999394844,
0.107475484252795));
#8784=CARTESIAN_POINT('Ctrl Pts',(0.809747234711808,-0.198712082533353,
0.0693141634661026));
#8785=CARTESIAN_POINT('Ctrl Pts',(0.814336113852846,-0.202908887997328,
0.0559106681449084));
#8786=CARTESIAN_POINT('Ctrl Pts',(0.820700905669331,-0.208554382393535,
0.028338825142918));
#8787=CARTESIAN_POINT('Ctrl Pts',(0.822447190954353,-0.21,0.0141630178371274));
#8788=CARTESIAN_POINT('Ctrl Pts',(0.822447190954353,-0.21,-0.0141630178371273));
#8789=CARTESIAN_POINT('Ctrl Pts',(0.820700905669331,-0.208554382393535,
-0.028338825142918));
#8790=CARTESIAN_POINT('Ctrl Pts',(0.814336113852846,-0.202908887997328,
-0.0559106681449083));
#8791=CARTESIAN_POINT('Ctrl Pts',(0.809747234711808,-0.198712082533353,
-0.0693141634661024));
#8792=CARTESIAN_POINT('Ctrl Pts',(0.7937414503193,-0.182517999394844,-0.107475484252795));
#8793=CARTESIAN_POINT('Ctrl Pts',(0.780239226177155,-0.166732877511574,
-0.130251970586776));
#8794=CARTESIAN_POINT('Ctrl Pts',(0.757108941035492,-0.130678518444188,
-0.166306329654162));
#8795=CARTESIAN_POINT('Ctrl Pts',(0.74560158587233,-0.107860332287474,-0.182341144032027));
#8796=CARTESIAN_POINT('Ctrl Pts',(0.729493747523555,-0.0563806217319965,
-0.204214038345313));
#8797=CARTESIAN_POINT('Ctrl Pts',(0.725,-0.0276636393226112,-0.21));
#8798=CARTESIAN_POINT('Ctrl Pts',(0.725,-9.71445146547012E-17,-0.21));
#8799=CARTESIAN_POINT('',(0.725,3.36777869765522E-17,0.42));
#8800=CARTESIAN_POINT('',(0.725,-3.36777869765522E-17,-1.1));
#8801=CARTESIAN_POINT('Origin',(1.,0.,0.42));
#8802=CARTESIAN_POINT('',(0.822447190954353,0.21,0.));
#8803=CARTESIAN_POINT('Ctrl Pts',(0.822447190954353,0.21,0.));
#8804=CARTESIAN_POINT('Ctrl Pts',(0.822447190954353,0.21,0.0141630178371274));
#8805=CARTESIAN_POINT('Ctrl Pts',(0.820700905669331,0.208554382393535,0.0283388251429181));
#8806=CARTESIAN_POINT('Ctrl Pts',(0.814336113852846,0.202908887997328,0.0559106681449084));
#8807=CARTESIAN_POINT('Ctrl Pts',(0.809747234711808,0.198712082533353,0.0693141634661024));
#8808=CARTESIAN_POINT('Ctrl Pts',(0.793741450319299,0.182517999394844,0.107475484252795));
#8809=CARTESIAN_POINT('Ctrl Pts',(0.780239226177155,0.166732877511574,0.130251970586776));
#8810=CARTESIAN_POINT('Ctrl Pts',(0.757108941035492,0.130678518444188,0.166306329654162));
#8811=CARTESIAN_POINT('Ctrl Pts',(0.74560158587233,0.107860332287474,0.182341144032027));
#8812=CARTESIAN_POINT('Ctrl Pts',(0.729493747523555,0.0563806217319964,
0.204214038345313));
#8813=CARTESIAN_POINT('Ctrl Pts',(0.725,0.0276636393226111,0.21));
#8814=CARTESIAN_POINT('Ctrl Pts',(0.725,2.77555756156289E-17,0.21));
#8815=CARTESIAN_POINT('Ctrl Pts',(0.725,-4.16333634234434E-17,-0.21));
#8816=CARTESIAN_POINT('Ctrl Pts',(0.725,0.027663639322611,-0.21));
#8817=CARTESIAN_POINT('Ctrl Pts',(0.729493747523555,0.0563806217319963,
-0.204214038345313));
#8818=CARTESIAN_POINT('Ctrl Pts',(0.74560158587233,0.107860332287473,-0.182341144032028));
#8819=CARTESIAN_POINT('Ctrl Pts',(0.757108941035492,0.130678518444188,-0.166306329654162));
#8820=CARTESIAN_POINT('Ctrl Pts',(0.780239226177155,0.166732877511574,-0.130251970586776));
#8821=CARTESIAN_POINT('Ctrl Pts',(0.793741450319299,0.182517999394844,-0.107475484252795));
#8822=CARTESIAN_POINT('Ctrl Pts',(0.809747234711808,0.198712082533353,-0.0693141634661025));
#8823=CARTESIAN_POINT('Ctrl Pts',(0.814336113852846,0.202908887997328,-0.0559106681449083));
#8824=CARTESIAN_POINT('Ctrl Pts',(0.820700905669331,0.208554382393535,-0.0283388251429181));
#8825=CARTESIAN_POINT('Ctrl Pts',(0.822447190954353,0.21,-0.0141630178371273));
#8826=CARTESIAN_POINT('Ctrl Pts',(0.822447190954353,0.21,6.93889390390723E-18));
#8827=CARTESIAN_POINT('Origin',(37.,0.,-1.1));
#8828=CARTESIAN_POINT('',(36.725,-3.3677786976552E-17,-0.42));
#8829=CARTESIAN_POINT('Origin',(37.,0.,-0.42));
#8830=CARTESIAN_POINT('',(36.725,2.05205711436755E-16,-0.21));
#8831=CARTESIAN_POINT('',(36.725,-3.3677786976552E-17,-1.1));
#8832=CARTESIAN_POINT('',(36.725,-7.0615321243557E-17,0.21));
#8833=CARTESIAN_POINT('Ctrl Pts',(36.725,-9.71445146547012E-17,0.21));
#8834=CARTESIAN_POINT('Ctrl Pts',(36.725,-0.0276636393226113,0.21));
#8835=CARTESIAN_POINT('Ctrl Pts',(36.7294937475236,-0.0563806217319973,
0.204214038345313));
#8836=CARTESIAN_POINT('Ctrl Pts',(36.7456015858723,-0.107860332287474,0.182341144032027));
#8837=CARTESIAN_POINT('Ctrl Pts',(36.7571089410355,-0.130678518444188,0.166306329654162));
#8838=CARTESIAN_POINT('Ctrl Pts',(36.7802392261772,-0.166732877511574,0.130251970586776));
#8839=CARTESIAN_POINT('Ctrl Pts',(36.7937414503193,-0.182517999394844,0.107475484252794));
#8840=CARTESIAN_POINT('Ctrl Pts',(36.8097472347118,-0.198712082533353,0.0693141634661021));
#8841=CARTESIAN_POINT('Ctrl Pts',(36.8143361138529,-0.202908887997328,0.0559106681449082));
#8842=CARTESIAN_POINT('Ctrl Pts',(36.8207009056693,-0.208554382393535,0.0283388251429169));
#8843=CARTESIAN_POINT('Ctrl Pts',(36.8224471909544,-0.21,0.0141630178371273));
#8844=CARTESIAN_POINT('Ctrl Pts',(36.8224471909544,-0.21,-0.0141630178371273));
#8845=CARTESIAN_POINT('Ctrl Pts',(36.8207009056693,-0.208554382393535,-0.0283388251429169));
#8846=CARTESIAN_POINT('Ctrl Pts',(36.8143361138529,-0.202908887997328,-0.0559106681449082));
#8847=CARTESIAN_POINT('Ctrl Pts',(36.8097472347118,-0.198712082533353,-0.0693141634661022));
#8848=CARTESIAN_POINT('Ctrl Pts',(36.7937414503193,-0.182517999394844,-0.107475484252794));
#8849=CARTESIAN_POINT('Ctrl Pts',(36.7802392261772,-0.166732877511574,-0.130251970586776));
#8850=CARTESIAN_POINT('Ctrl Pts',(36.7571089410355,-0.130678518444188,-0.166306329654162));
#8851=CARTESIAN_POINT('Ctrl Pts',(36.7456015858723,-0.107860332287474,-0.182341144032027));
#8852=CARTESIAN_POINT('Ctrl Pts',(36.7294937475236,-0.0563806217319974,
-0.204214038345313));
#8853=CARTESIAN_POINT('Ctrl Pts',(36.725,-0.0276636393226115,-0.21));
#8854=CARTESIAN_POINT('Ctrl Pts',(36.725,-2.84494650060196E-16,-0.21));
#8855=CARTESIAN_POINT('',(36.725,3.3677786976552E-17,0.42));
#8856=CARTESIAN_POINT('',(36.725,-3.3677786976552E-17,-1.1));
#8857=CARTESIAN_POINT('Origin',(37.,0.,0.42));
#8858=CARTESIAN_POINT('',(36.8224471909543,0.21,1.49186218934005E-16));
#8859=CARTESIAN_POINT('Ctrl Pts',(36.8224471909543,0.21,1.49186218934005E-16));
#8860=CARTESIAN_POINT('Ctrl Pts',(36.8224471909543,0.21,0.0141630178371275));
#8861=CARTESIAN_POINT('Ctrl Pts',(36.8207009056693,0.208554382393535,0.028338825142917));
#8862=CARTESIAN_POINT('Ctrl Pts',(36.8143361138529,0.202908887997328,0.0559106681449084));
#8863=CARTESIAN_POINT('Ctrl Pts',(36.8097472347118,0.198712082533353,0.0693141634661022));
#8864=CARTESIAN_POINT('Ctrl Pts',(36.7937414503193,0.182517999394844,0.107475484252794));
#8865=CARTESIAN_POINT('Ctrl Pts',(36.7802392261772,0.166732877511574,0.130251970586776));
#8866=CARTESIAN_POINT('Ctrl Pts',(36.7571089410355,0.130678518444188,0.166306329654162));
#8867=CARTESIAN_POINT('Ctrl Pts',(36.7456015858723,0.107860332287474,0.182341144032027));
#8868=CARTESIAN_POINT('Ctrl Pts',(36.7294937475236,0.0563806217319973,0.204214038345313));
#8869=CARTESIAN_POINT('Ctrl Pts',(36.725,0.0276636393226112,0.21));
#8870=CARTESIAN_POINT('Ctrl Pts',(36.725,2.08166817117217E-17,0.21));
#8871=CARTESIAN_POINT('Ctrl Pts',(36.725,2.08166817117217E-16,-0.21));
#8872=CARTESIAN_POINT('Ctrl Pts',(36.725,0.0276636393226114,-0.21));
#8873=CARTESIAN_POINT('Ctrl Pts',(36.7294937475236,0.0563806217319972,-0.204214038345313));
#8874=CARTESIAN_POINT('Ctrl Pts',(36.7456015858723,0.107860332287474,-0.182341144032027));
#8875=CARTESIAN_POINT('Ctrl Pts',(36.7571089410355,0.130678518444188,-0.166306329654162));
#8876=CARTESIAN_POINT('Ctrl Pts',(36.7802392261772,0.166732877511574,-0.130251970586776));
#8877=CARTESIAN_POINT('Ctrl Pts',(36.7937414503193,0.182517999394844,-0.107475484252794));
#8878=CARTESIAN_POINT('Ctrl Pts',(36.8097472347118,0.198712082533353,-0.0693141634661023));
#8879=CARTESIAN_POINT('Ctrl Pts',(36.8143361138529,0.202908887997328,-0.0559106681449084));
#8880=CARTESIAN_POINT('Ctrl Pts',(36.8207009056693,0.208554382393535,-0.028338825142917));
#8881=CARTESIAN_POINT('Ctrl Pts',(36.8224471909543,0.21,-0.0141630178371273));
#8882=CARTESIAN_POINT('Ctrl Pts',(36.8224471909543,0.21,5.55111512312578E-17));
#8883=CARTESIAN_POINT('',(37.1775528090456,0.21,-1.73472347597681E-18));
#8884=CARTESIAN_POINT('',(37.275,-4.32661872577435E-16,0.21));
#8885=CARTESIAN_POINT('Ctrl Pts',(37.1775528090456,0.21,-1.73472347597681E-18));
#8886=CARTESIAN_POINT('Ctrl Pts',(37.1775528090456,0.21,-0.0141630178371273));
#8887=CARTESIAN_POINT('Ctrl Pts',(37.1792990943307,0.208554382393535,-0.028338825142917));
#8888=CARTESIAN_POINT('Ctrl Pts',(37.1856638861471,0.202908887997328,-0.0559106681449084));
#8889=CARTESIAN_POINT('Ctrl Pts',(37.1902527652882,0.198712082533353,-0.0693141634661023));
#8890=CARTESIAN_POINT('Ctrl Pts',(37.2062585496807,0.182517999394844,-0.107475484252794));
#8891=CARTESIAN_POINT('Ctrl Pts',(37.2197607738228,0.166732877511574,-0.130251970586776));
#8892=CARTESIAN_POINT('Ctrl Pts',(37.2428910589645,0.130678518444188,-0.166306329654162));
#8893=CARTESIAN_POINT('Ctrl Pts',(37.2543984141277,0.107860332287474,-0.182341144032027));
#8894=CARTESIAN_POINT('Ctrl Pts',(37.2705062524764,0.0563806217319972,-0.204214038345313));
#8895=CARTESIAN_POINT('Ctrl Pts',(37.275,0.0276636393226112,-0.21));
#8896=CARTESIAN_POINT('Ctrl Pts',(37.275,-0.0276636393226113,-0.21));
#8897=CARTESIAN_POINT('Ctrl Pts',(37.2705062524764,-0.0563806217319974,
-0.204214038345313));
#8898=CARTESIAN_POINT('Ctrl Pts',(37.2543984141277,-0.107860332287474,-0.182341144032027));
#8899=CARTESIAN_POINT('Ctrl Pts',(37.2428910589645,-0.130678518444188,-0.166306329654162));
#8900=CARTESIAN_POINT('Ctrl Pts',(37.2197607738228,-0.166732877511574,-0.130251970586776));
#8901=CARTESIAN_POINT('Ctrl Pts',(37.2062585496807,-0.182517999394844,-0.107475484252794));
#8902=CARTESIAN_POINT('Ctrl Pts',(37.1902527652882,-0.198712082533353,-0.0693141634661022));
#8903=CARTESIAN_POINT('Ctrl Pts',(37.1856638861471,-0.202908887997328,-0.0559106681449083));
#8904=CARTESIAN_POINT('Ctrl Pts',(37.1792990943307,-0.208554382393535,-0.028338825142917));
#8905=CARTESIAN_POINT('Ctrl Pts',(37.1775528090456,-0.21,-0.0141630178371273));
#8906=CARTESIAN_POINT('Ctrl Pts',(37.1775528090456,-0.21,0.0141630178371273));
#8907=CARTESIAN_POINT('Ctrl Pts',(37.1792990943307,-0.208554382393535,0.028338825142917));
#8908=CARTESIAN_POINT('Ctrl Pts',(37.1856638861471,-0.202908887997328,0.0559106681449084));
#8909=CARTESIAN_POINT('Ctrl Pts',(37.1902527652882,-0.198712082533353,0.0693141634661023));
#8910=CARTESIAN_POINT('Ctrl Pts',(37.2062585496807,-0.182517999394844,0.107475484252794));
#8911=CARTESIAN_POINT('Ctrl Pts',(37.2197607738228,-0.166732877511574,0.130251970586776));
#8912=CARTESIAN_POINT('Ctrl Pts',(37.2428910589645,-0.130678518444188,0.166306329654162));
#8913=CARTESIAN_POINT('Ctrl Pts',(37.2543984141277,-0.107860332287474,0.182341144032027));
#8914=CARTESIAN_POINT('Ctrl Pts',(37.2705062524764,-0.0563806217319973,
0.204214038345313));
#8915=CARTESIAN_POINT('Ctrl Pts',(37.275,-0.0276636393226111,0.21));
#8916=CARTESIAN_POINT('Ctrl Pts',(37.275,1.04083408558608E-16,0.21));
#8917=CARTESIAN_POINT('Ctrl Pts',(37.275,-7.97972798949331E-17,0.21));
#8918=CARTESIAN_POINT('Ctrl Pts',(37.275,0.0276636393226111,0.21));
#8919=CARTESIAN_POINT('Ctrl Pts',(37.2705062524764,0.0563806217319973,0.204214038345313));
#8920=CARTESIAN_POINT('Ctrl Pts',(37.2543984141277,0.107860332287474,0.182341144032027));
#8921=CARTESIAN_POINT('Ctrl Pts',(37.2428910589645,0.130678518444188,0.166306329654162));
#8922=CARTESIAN_POINT('Ctrl Pts',(37.2197607738228,0.166732877511574,0.130251970586776));
#8923=CARTESIAN_POINT('Ctrl Pts',(37.2062585496807,0.182517999394844,0.107475484252794));
#8924=CARTESIAN_POINT('Ctrl Pts',(37.1902527652882,0.198712082533353,0.0693141634661022));
#8925=CARTESIAN_POINT('Ctrl Pts',(37.1856638861471,0.202908887997328,0.0559106681449083));
#8926=CARTESIAN_POINT('Ctrl Pts',(37.1792990943307,0.208554382393535,0.028338825142917));
#8927=CARTESIAN_POINT('Ctrl Pts',(37.1775528090457,0.21,0.0141630178371273));
#8928=CARTESIAN_POINT('Ctrl Pts',(37.1775528090457,0.21,-1.04083408558608E-17));
#8929=CARTESIAN_POINT('Origin',(-0.1,0.,0.));
#8930=CARTESIAN_POINT('',(-0.1,-2.57175827820944E-17,0.21));
#8931=CARTESIAN_POINT('Origin',(-0.1,0.,0.));
#8932=CARTESIAN_POINT('',(0.,-2.57175827820944E-17,0.21));
#8933=CARTESIAN_POINT('Origin',(0.,0.,0.));
#8934=CARTESIAN_POINT('',(-0.1,-2.57175827820944E-17,0.21));
#8935=CARTESIAN_POINT('Origin',(-0.1,0.82,-0.3));
#8936=CARTESIAN_POINT('',(0.,0.82,-0.3));
#8937=CARTESIAN_POINT('',(0.,1.,-0.3));
#8938=CARTESIAN_POINT('',(0.,0.41,-0.3));
#8939=CARTESIAN_POINT('',(40.,0.82,-0.3));
#8940=CARTESIAN_POINT('',(-0.1,0.82,-0.3));
#8941=CARTESIAN_POINT('',(40.,1.,-0.3));
#8942=CARTESIAN_POINT('',(40.,0.41,-0.3));
#8943=CARTESIAN_POINT('',(-0.05,1.,-0.3));
#8944=CARTESIAN_POINT('Origin',(-0.1,0.82,-0.55));
#8945=CARTESIAN_POINT('',(0.,0.82,-0.55));
#8946=CARTESIAN_POINT('',(0.,0.82,-0.275));
#8947=CARTESIAN_POINT('',(40.,0.82,-0.55));
#8948=CARTESIAN_POINT('',(-0.1,0.82,-0.55));
#8949=CARTESIAN_POINT('',(40.,0.82,-0.275));
#8950=CARTESIAN_POINT('Origin',(-0.1,0.67,-0.55));
#8951=CARTESIAN_POINT('',(0.,0.67,-0.55));
#8952=CARTESIAN_POINT('',(0.,0.335,-0.55));
#8953=CARTESIAN_POINT('',(40.,0.67,-0.55));
#8954=CARTESIAN_POINT('',(-0.1,0.67,-0.55));
#8955=CARTESIAN_POINT('',(40.,0.335,-0.55));
#8956=CARTESIAN_POINT('Origin',(-0.1,0.42,-0.3));
#8957=CARTESIAN_POINT('',(0.,0.42,-0.3));
#8958=CARTESIAN_POINT('',(0.,0.24,-0.12));
#8959=CARTESIAN_POINT('',(40.,0.42,-0.3));
#8960=CARTESIAN_POINT('',(-0.1,0.42,-0.3));
#8961=CARTESIAN_POINT('',(40.,0.24,-0.12));
#8962=CARTESIAN_POINT('Origin',(-0.1,0.42,0.3));
#8963=CARTESIAN_POINT('',(0.,0.42,0.3));
#8964=CARTESIAN_POINT('',(0.,0.42,0.15));
#8965=CARTESIAN_POINT('',(40.,0.42,0.3));
#8966=CARTESIAN_POINT('',(-0.1,0.42,0.3));
#8967=CARTESIAN_POINT('',(40.,0.42,0.15));
#8968=CARTESIAN_POINT('Origin',(-0.1,0.67,0.55));
#8969=CARTESIAN_POINT('',(0.,0.67,0.55));
#8970=CARTESIAN_POINT('',(6.93889390390723E-18,0.365,0.245));
#8971=CARTESIAN_POINT('',(40.,0.67,0.55));
#8972=CARTESIAN_POINT('',(-0.1,0.67,0.55));
#8973=CARTESIAN_POINT('',(40.,0.365,0.245));
#8974=CARTESIAN_POINT('Origin',(-0.1,0.82,0.55));
#8975=CARTESIAN_POINT('',(0.,0.82,0.55));
#8976=CARTESIAN_POINT('',(0.,0.41,0.55));
#8977=CARTESIAN_POINT('',(40.,0.82,0.55));
#8978=CARTESIAN_POINT('',(-0.1,0.82,0.55));
#8979=CARTESIAN_POINT('',(40.,0.41,0.55));
#8980=CARTESIAN_POINT('Origin',(-0.1,0.82,0.3));
#8981=CARTESIAN_POINT('',(0.,0.82,0.3));
#8982=CARTESIAN_POINT('',(0.,0.82,0.15));
#8983=CARTESIAN_POINT('',(40.,0.82,0.3));
#8984=CARTESIAN_POINT('',(-0.1,0.82,0.3));
#8985=CARTESIAN_POINT('',(40.,0.82,0.15));
#8986=CARTESIAN_POINT('Origin',(-0.1,1.05,0.3));
#8987=CARTESIAN_POINT('',(0.,1.,0.3));
#8988=CARTESIAN_POINT('',(0.,0.525,0.3));
#8989=CARTESIAN_POINT('',(40.,1.,0.3));
#8990=CARTESIAN_POINT('',(-0.05,1.,0.3));
#8991=CARTESIAN_POINT('',(40.,0.525,0.3));
#8992=CARTESIAN_POINT('Origin',(-0.1,-0.3,-0.82));
#8993=CARTESIAN_POINT('',(0.,-0.3,-0.82));
#8994=CARTESIAN_POINT('',(0.,-0.3,-1.));
#8995=CARTESIAN_POINT('',(0.,-0.3,-0.41));
#8996=CARTESIAN_POINT('',(40.,-0.3,-0.82));
#8997=CARTESIAN_POINT('',(-0.1,-0.3,-0.82));
#8998=CARTESIAN_POINT('',(40.,-0.3,-1.));
#8999=CARTESIAN_POINT('',(40.,-0.3,-0.41));
#9000=CARTESIAN_POINT('',(-0.05,-0.3,-1.));
#9001=CARTESIAN_POINT('Origin',(-0.1,-0.55,-0.82));
#9002=CARTESIAN_POINT('',(0.,-0.55,-0.82));
#9003=CARTESIAN_POINT('',(0.,-0.275,-0.82));
#9004=CARTESIAN_POINT('',(40.,-0.55,-0.82));
#9005=CARTESIAN_POINT('',(-0.1,-0.55,-0.82));
#9006=CARTESIAN_POINT('',(40.,-0.275,-0.82));
#9007=CARTESIAN_POINT('Origin',(-0.1,-0.55,-0.67));
#9008=CARTESIAN_POINT('',(0.,-0.55,-0.67));
#9009=CARTESIAN_POINT('',(0.,-0.55,-0.335));
#9010=CARTESIAN_POINT('',(40.,-0.55,-0.67));
#9011=CARTESIAN_POINT('',(-0.1,-0.55,-0.67));
#9012=CARTESIAN_POINT('',(40.,-0.55,-0.335));
#9013=CARTESIAN_POINT('Origin',(-0.1,-0.3,-0.42));
#9014=CARTESIAN_POINT('',(0.,-0.3,-0.42));
#9015=CARTESIAN_POINT('',(0.,-0.12,-0.24));
#9016=CARTESIAN_POINT('',(40.,-0.3,-0.42));
#9017=CARTESIAN_POINT('',(-0.1,-0.3,-0.42));
#9018=CARTESIAN_POINT('',(40.,-0.12,-0.24));
#9019=CARTESIAN_POINT('Origin',(-0.1,0.3,-0.42));
#9020=CARTESIAN_POINT('',(0.,0.3,-0.42));
#9021=CARTESIAN_POINT('',(0.,0.15,-0.42));
#9022=CARTESIAN_POINT('',(40.,0.3,-0.42));
#9023=CARTESIAN_POINT('',(-0.1,0.3,-0.42));
#9024=CARTESIAN_POINT('',(40.,0.15,-0.42));
#9025=CARTESIAN_POINT('Origin',(-0.1,0.55,-0.67));
#9026=CARTESIAN_POINT('',(0.,0.55,-0.67));
#9027=CARTESIAN_POINT('',(0.,0.245,-0.365));
#9028=CARTESIAN_POINT('',(40.,0.55,-0.67));
#9029=CARTESIAN_POINT('',(-0.1,0.55,-0.67));
#9030=CARTESIAN_POINT('',(40.,0.245,-0.365));
#9031=CARTESIAN_POINT('Origin',(-0.1,0.55,-0.82));
#9032=CARTESIAN_POINT('',(0.,0.55,-0.82));
#9033=CARTESIAN_POINT('',(0.,0.55,-0.41));
#9034=CARTESIAN_POINT('',(40.,0.55,-0.82));
#9035=CARTESIAN_POINT('',(-0.1,0.55,-0.82));
#9036=CARTESIAN_POINT('',(40.,0.55,-0.41));
#9037=CARTESIAN_POINT('Origin',(-0.1,0.3,-0.82));
#9038=CARTESIAN_POINT('',(0.,0.3,-0.82));
#9039=CARTESIAN_POINT('',(0.,0.15,-0.82));
#9040=CARTESIAN_POINT('',(40.,0.3,-0.82));
#9041=CARTESIAN_POINT('',(-0.1,0.3,-0.82));
#9042=CARTESIAN_POINT('',(40.,0.15,-0.82));
#9043=CARTESIAN_POINT('Origin',(-0.1,0.3,-1.05));
#9044=CARTESIAN_POINT('',(0.,0.3,-1.));
#9045=CARTESIAN_POINT('',(0.,0.3,-0.525));
#9046=CARTESIAN_POINT('',(40.,0.3,-1.));
#9047=CARTESIAN_POINT('',(-0.05,0.3,-1.));
#9048=CARTESIAN_POINT('',(40.,0.3,-0.525));
#9049=CARTESIAN_POINT('Origin',(-0.1,-0.82,0.3));
#9050=CARTESIAN_POINT('',(0.,-0.82,0.3));
#9051=CARTESIAN_POINT('',(0.,-1.,0.3));
#9052=CARTESIAN_POINT('',(0.,-0.41,0.3));
#9053=CARTESIAN_POINT('',(40.,-0.82,0.3));
#9054=CARTESIAN_POINT('',(-0.1,-0.82,0.3));
#9055=CARTESIAN_POINT('',(40.,-1.,0.3));
#9056=CARTESIAN_POINT('',(40.,-0.41,0.3));
#9057=CARTESIAN_POINT('',(-0.05,-1.,0.3));
#9058=CARTESIAN_POINT('Origin',(-0.1,-0.82,0.55));
#9059=CARTESIAN_POINT('',(0.,-0.82,0.55));
#9060=CARTESIAN_POINT('',(0.,-0.82,0.275));
#9061=CARTESIAN_POINT('',(40.,-0.82,0.55));
#9062=CARTESIAN_POINT('',(-0.1,-0.82,0.55));
#9063=CARTESIAN_POINT('',(40.,-0.82,0.275));
#9064=CARTESIAN_POINT('Origin',(-0.1,-0.67,0.55));
#9065=CARTESIAN_POINT('',(0.,-0.67,0.55));
#9066=CARTESIAN_POINT('',(0.,-0.335,0.55));
#9067=CARTESIAN_POINT('',(40.,-0.67,0.55));
#9068=CARTESIAN_POINT('',(-0.1,-0.67,0.55));
#9069=CARTESIAN_POINT('',(40.,-0.335,0.55));
#9070=CARTESIAN_POINT('Origin',(-0.1,-0.42,0.3));
#9071=CARTESIAN_POINT('',(0.,-0.42,0.3));
#9072=CARTESIAN_POINT('',(-6.93889390390723E-18,-0.24,0.12));
#9073=CARTESIAN_POINT('',(40.,-0.42,0.3));
#9074=CARTESIAN_POINT('',(-0.1,-0.42,0.3));
#9075=CARTESIAN_POINT('',(40.,-0.24,0.12));
#9076=CARTESIAN_POINT('Origin',(-0.1,-0.42,-0.3));
#9077=CARTESIAN_POINT('',(0.,-0.42,-0.3));
#9078=CARTESIAN_POINT('',(0.,-0.42,-0.15));
#9079=CARTESIAN_POINT('',(40.,-0.42,-0.3));
#9080=CARTESIAN_POINT('',(-0.1,-0.42,-0.3));
#9081=CARTESIAN_POINT('',(40.,-0.42,-0.15));
#9082=CARTESIAN_POINT('Origin',(-0.1,-0.67,-0.55));
#9083=CARTESIAN_POINT('',(0.,-0.67,-0.55));
#9084=CARTESIAN_POINT('',(0.,-0.365,-0.245));
#9085=CARTESIAN_POINT('',(40.,-0.67,-0.55));
#9086=CARTESIAN_POINT('',(-0.1,-0.67,-0.55));
#9087=CARTESIAN_POINT('',(40.,-0.365,-0.245));
#9088=CARTESIAN_POINT('Origin',(-0.1,-0.82,-0.55));
#9089=CARTESIAN_POINT('',(0.,-0.82,-0.55));
#9090=CARTESIAN_POINT('',(0.,-0.41,-0.55));
#9091=CARTESIAN_POINT('',(40.,-0.82,-0.55));
#9092=CARTESIAN_POINT('',(-0.1,-0.82,-0.55));
#9093=CARTESIAN_POINT('',(40.,-0.41,-0.55));
#9094=CARTESIAN_POINT('Origin',(-0.1,-0.82,-0.3));
#9095=CARTESIAN_POINT('',(0.,-0.82,-0.3));
#9096=CARTESIAN_POINT('',(0.,-0.82,-0.15));
#9097=CARTESIAN_POINT('',(40.,-0.82,-0.3));
#9098=CARTESIAN_POINT('',(-0.1,-0.82,-0.3));
#9099=CARTESIAN_POINT('',(40.,-0.82,-0.15));
#9100=CARTESIAN_POINT('Origin',(-0.1,-1.05,-0.3));
#9101=CARTESIAN_POINT('',(0.,-1.,-0.3));
#9102=CARTESIAN_POINT('',(0.,-0.525,-0.3));
#9103=CARTESIAN_POINT('',(40.,-1.,-0.3));
#9104=CARTESIAN_POINT('',(-0.05,-1.,-0.3));
#9105=CARTESIAN_POINT('',(40.,-0.525,-0.3));
#9106=CARTESIAN_POINT('Origin',(-0.1,0.3,0.82));
#9107=CARTESIAN_POINT('',(0.,0.3,0.82));
#9108=CARTESIAN_POINT('',(0.,0.3,1.));
#9109=CARTESIAN_POINT('',(0.,0.3,0.41));
#9110=CARTESIAN_POINT('',(40.,0.3,0.82));
#9111=CARTESIAN_POINT('',(-0.1,0.3,0.82));
#9112=CARTESIAN_POINT('',(40.,0.3,1.));
#9113=CARTESIAN_POINT('',(40.,0.3,0.41));
#9114=CARTESIAN_POINT('',(-0.05,0.3,1.));
#9115=CARTESIAN_POINT('Origin',(-0.1,0.55,0.82));
#9116=CARTESIAN_POINT('',(0.,0.55,0.82));
#9117=CARTESIAN_POINT('',(0.,0.275,0.82));
#9118=CARTESIAN_POINT('',(40.,0.55,0.82));
#9119=CARTESIAN_POINT('',(-0.1,0.55,0.82));
#9120=CARTESIAN_POINT('',(40.,0.275,0.82));
#9121=CARTESIAN_POINT('Origin',(-0.1,0.55,0.67));
#9122=CARTESIAN_POINT('',(0.,0.55,0.67));
#9123=CARTESIAN_POINT('',(0.,0.55,0.335));
#9124=CARTESIAN_POINT('',(40.,0.55,0.67));
#9125=CARTESIAN_POINT('',(-0.1,0.55,0.67));
#9126=CARTESIAN_POINT('',(40.,0.55,0.335));
#9127=CARTESIAN_POINT('Origin',(-0.1,0.3,0.42));
#9128=CARTESIAN_POINT('',(0.,0.3,0.42));
#9129=CARTESIAN_POINT('',(6.93889390390723E-18,0.12,0.24));
#9130=CARTESIAN_POINT('',(40.,0.3,0.42));
#9131=CARTESIAN_POINT('',(-0.1,0.3,0.42));
#9132=CARTESIAN_POINT('',(40.,0.12,0.24));
#9133=CARTESIAN_POINT('Origin',(-0.1,-0.3,0.42));
#9134=CARTESIAN_POINT('',(0.,-0.3,0.42));
#9135=CARTESIAN_POINT('',(0.,-0.15,0.42));
#9136=CARTESIAN_POINT('',(40.,-0.3,0.42));
#9137=CARTESIAN_POINT('',(-0.1,-0.3,0.42));
#9138=CARTESIAN_POINT('',(40.,-0.15,0.42));
#9139=CARTESIAN_POINT('Origin',(-0.1,-0.55,0.67));
#9140=CARTESIAN_POINT('',(0.,-0.55,0.67));
#9141=CARTESIAN_POINT('',(6.93889390390723E-18,-0.245,0.365));
#9142=CARTESIAN_POINT('',(40.,-0.55,0.67));
#9143=CARTESIAN_POINT('',(-0.1,-0.55,0.67));
#9144=CARTESIAN_POINT('',(40.,-0.245,0.365));
#9145=CARTESIAN_POINT('Origin',(-0.1,-0.55,0.82));
#9146=CARTESIAN_POINT('',(0.,-0.55,0.82));
#9147=CARTESIAN_POINT('',(0.,-0.55,0.41));
#9148=CARTESIAN_POINT('',(40.,-0.55,0.82));
#9149=CARTESIAN_POINT('',(-0.1,-0.55,0.82));
#9150=CARTESIAN_POINT('',(40.,-0.55,0.41));
#9151=CARTESIAN_POINT('Origin',(-0.1,-0.3,0.82));
#9152=CARTESIAN_POINT('',(0.,-0.3,0.82));
#9153=CARTESIAN_POINT('',(0.,-0.15,0.82));
#9154=CARTESIAN_POINT('',(40.,-0.3,0.82));
#9155=CARTESIAN_POINT('',(-0.1,-0.3,0.82));
#9156=CARTESIAN_POINT('',(40.,-0.15,0.82));
#9157=CARTESIAN_POINT('Origin',(-0.1,-0.3,1.05));
#9158=CARTESIAN_POINT('',(0.,-0.3,1.));
#9159=CARTESIAN_POINT('',(0.,-0.3,0.525));
#9160=CARTESIAN_POINT('',(40.,-0.3,1.));
#9161=CARTESIAN_POINT('',(-0.05,-0.3,1.));
#9162=CARTESIAN_POINT('',(40.,-0.3,0.525));
#9163=CARTESIAN_POINT('Origin',(-0.1,0.,0.));
#9164=CARTESIAN_POINT('',(40.,2.57175827820944E-17,0.21));
#9165=CARTESIAN_POINT('',(-0.1,-2.57175827820944E-17,0.21));
#9166=CARTESIAN_POINT('Origin',(40.,0.,0.));
#9167=CARTESIAN_POINT('Origin',(0.,1.,-1.));
#9168=CARTESIAN_POINT('',(0.,1.,1.));
#9169=CARTESIAN_POINT('',(0.,1.,-1.));
#9170=CARTESIAN_POINT('',(40.,1.,1.));
#9171=CARTESIAN_POINT('',(0.,1.,1.));
#9172=CARTESIAN_POINT('',(40.,1.,-1.));
#9173=CARTESIAN_POINT('Origin',(0.,1.,-1.));
#9174=CARTESIAN_POINT('',(40.,1.,-1.));
#9175=CARTESIAN_POINT('',(40.,1.,-1.));
#9176=CARTESIAN_POINT('',(0.,1.,-1.));
#9177=CARTESIAN_POINT('',(0.,1.,-1.));
#9178=CARTESIAN_POINT('',(0.,1.,-1.));
#9179=CARTESIAN_POINT('Origin',(0.,-1.,-1.));
#9180=CARTESIAN_POINT('',(0.,-1.,-1.));
#9181=CARTESIAN_POINT('',(40.,-1.,-1.));
#9182=CARTESIAN_POINT('Origin',(0.,-1.,-1.));
#9183=CARTESIAN_POINT('',(40.,-1.,-1.));
#9184=CARTESIAN_POINT('',(40.,-1.,-1.));
#9185=CARTESIAN_POINT('',(0.,-1.,-1.));
#9186=CARTESIAN_POINT('',(0.,-1.,-1.));
#9187=CARTESIAN_POINT('',(0.,-1.,-1.));
#9188=CARTESIAN_POINT('Origin',(0.,-1.,1.));
#9189=CARTESIAN_POINT('',(0.,-1.,1.));
#9190=CARTESIAN_POINT('',(40.,-1.,1.));
#9191=CARTESIAN_POINT('Origin',(0.,-1.,1.));
#9192=CARTESIAN_POINT('',(40.,-1.,1.));
#9193=CARTESIAN_POINT('',(40.,-1.,1.));
#9194=CARTESIAN_POINT('',(0.,-1.,1.));
#9195=CARTESIAN_POINT('',(0.,-1.,1.));
#9196=CARTESIAN_POINT('',(0.,-1.,1.));
#9197=CARTESIAN_POINT('Origin',(0.,1.,1.));
#9198=CARTESIAN_POINT('',(0.,1.,1.));
#9199=CARTESIAN_POINT('',(40.,1.,1.));
#9200=CARTESIAN_POINT('Origin',(0.,1.,1.));
#9201=CARTESIAN_POINT('',(40.,1.,1.));
#9202=CARTESIAN_POINT('',(0.,1.,1.));
#9203=CARTESIAN_POINT('Origin',(40.,0.,0.));
#9204=CARTESIAN_POINT('Origin',(0.,0.,0.));
#9205=CARTESIAN_POINT('',(0.,0.,0.));
#9206=CARTESIAN_POINT('Origin',(36.,0.,0.));
#9207=CARTESIAN_POINT('',(36.,0.3,0.82));
#9208=CARTESIAN_POINT('',(36.,0.3,1.));
#9209=CARTESIAN_POINT('',(36.,0.3,0.41));
#9210=CARTESIAN_POINT('',(36.,0.55,0.82));
#9211=CARTESIAN_POINT('',(36.,0.275,0.82));
#9212=CARTESIAN_POINT('',(36.,0.55,0.67));
#9213=CARTESIAN_POINT('',(36.,0.55,0.335));
#9214=CARTESIAN_POINT('',(36.,0.3,0.42));
#9215=CARTESIAN_POINT('',(36.,0.12,0.24));
#9216=CARTESIAN_POINT('',(36.,-0.3,0.42));
#9217=CARTESIAN_POINT('',(36.,-0.15,0.42));
#9218=CARTESIAN_POINT('',(36.,-0.55,0.67));
#9219=CARTESIAN_POINT('',(36.,-0.245,0.365));
#9220=CARTESIAN_POINT('',(36.,-0.55,0.82));
#9221=CARTESIAN_POINT('',(36.,-0.55,0.41));
#9222=CARTESIAN_POINT('',(36.,-0.3,0.82));
#9223=CARTESIAN_POINT('',(36.,-0.15,0.82));
#9224=CARTESIAN_POINT('',(36.,-0.3,1.));
#9225=CARTESIAN_POINT('',(36.,-0.3,0.525));
#9226=CARTESIAN_POINT('',(36.,-1.,1.));
#9227=CARTESIAN_POINT('',(36.,0.5,1.));
#9228=CARTESIAN_POINT('',(36.,-1.,0.3));
#9229=CARTESIAN_POINT('',(36.,-1.,0.5));
#9230=CARTESIAN_POINT('',(36.,-0.82,0.3));
#9231=CARTESIAN_POINT('',(36.,-0.41,0.3));
#9232=CARTESIAN_POINT('',(36.,-0.82,0.55));
#9233=CARTESIAN_POINT('',(36.,-0.82,0.275));
#9234=CARTESIAN_POINT('',(36.,-0.67,0.55));
#9235=CARTESIAN_POINT('',(36.,-0.335,0.55));
#9236=CARTESIAN_POINT('',(36.,-0.42,0.3));
#9237=CARTESIAN_POINT('',(36.,-0.24,0.12));
#9238=CARTESIAN_POINT('',(36.,-0.42,-0.3));
#9239=CARTESIAN_POINT('',(36.,-0.42,-0.15));
#9240=CARTESIAN_POINT('',(36.,-0.67,-0.55));
#9241=CARTESIAN_POINT('',(36.,-0.365,-0.245));
#9242=CARTESIAN_POINT('',(36.,-0.82,-0.55));
#9243=CARTESIAN_POINT('',(36.,-0.41,-0.55));
#9244=CARTESIAN_POINT('',(36.,-0.82,-0.3));
#9245=CARTESIAN_POINT('',(36.,-0.82,-0.15));
#9246=CARTESIAN_POINT('',(36.,-1.,-0.3));
#9247=CARTESIAN_POINT('',(36.,-0.525,-0.3));
#9248=CARTESIAN_POINT('',(36.,-1.,-1.));
#9249=CARTESIAN_POINT('',(36.,-1.,0.5));
#9250=CARTESIAN_POINT('',(36.,-0.3,-1.));
#9251=CARTESIAN_POINT('',(36.,-0.5,-1.));
#9252=CARTESIAN_POINT('',(36.,-0.3,-0.82));
#9253=CARTESIAN_POINT('',(36.,-0.3,-0.41));
#9254=CARTESIAN_POINT('',(36.,-0.55,-0.82));
#9255=CARTESIAN_POINT('',(36.,-0.275,-0.82));
#9256=CARTESIAN_POINT('',(36.,-0.55,-0.67));
#9257=CARTESIAN_POINT('',(36.,-0.55,-0.335));
#9258=CARTESIAN_POINT('',(36.,-0.3,-0.42));
#9259=CARTESIAN_POINT('',(36.,-0.12,-0.24));
#9260=CARTESIAN_POINT('',(36.,0.3,-0.42));
#9261=CARTESIAN_POINT('',(36.,0.15,-0.42));
#9262=CARTESIAN_POINT('',(36.,0.55,-0.67));
#9263=CARTESIAN_POINT('',(36.,0.245,-0.365));
#9264=CARTESIAN_POINT('',(36.,0.55,-0.82));
#9265=CARTESIAN_POINT('',(36.,0.55,-0.41));
#9266=CARTESIAN_POINT('',(36.,0.3,-0.82));
#9267=CARTESIAN_POINT('',(36.,0.15,-0.82));
#9268=CARTESIAN_POINT('',(36.,0.3,-1.));
#9269=CARTESIAN_POINT('',(36.,0.3,-0.525));
#9270=CARTESIAN_POINT('',(36.,1.,-1.));
#9271=CARTESIAN_POINT('',(36.,-0.5,-1.));
#9272=CARTESIAN_POINT('',(36.,1.,-0.3));
#9273=CARTESIAN_POINT('',(36.,1.,-0.5));
#9274=CARTESIAN_POINT('',(36.,0.82,-0.3));
#9275=CARTESIAN_POINT('',(36.,0.41,-0.3));
#9276=CARTESIAN_POINT('',(36.,0.82,-0.55));
#9277=CARTESIAN_POINT('',(36.,0.82,-0.275));
#9278=CARTESIAN_POINT('',(36.,0.67,-0.55));
#9279=CARTESIAN_POINT('',(36.,0.335,-0.55));
#9280=CARTESIAN_POINT('',(36.,0.42,-0.3));
#9281=CARTESIAN_POINT('',(36.,0.24,-0.12));
#9282=CARTESIAN_POINT('',(36.,0.42,0.3));
#9283=CARTESIAN_POINT('',(36.,0.42,0.15));
#9284=CARTESIAN_POINT('',(36.,0.67,0.55));
#9285=CARTESIAN_POINT('',(36.,0.365,0.245));
#9286=CARTESIAN_POINT('',(36.,0.82,0.55));
#9287=CARTESIAN_POINT('',(36.,0.41,0.55));
#9288=CARTESIAN_POINT('',(36.,0.82,0.3));
#9289=CARTESIAN_POINT('',(36.,0.82,0.15));
#9290=CARTESIAN_POINT('',(36.,1.,0.3));
#9291=CARTESIAN_POINT('',(36.,0.525,0.3));
#9292=CARTESIAN_POINT('',(36.,1.,1.));
#9293=CARTESIAN_POINT('',(36.,1.,-0.5));
#9294=CARTESIAN_POINT('',(36.,0.5,1.));
#9295=CARTESIAN_POINT('',(36.,-2.57175827820944E-17,0.21));
#9296=CARTESIAN_POINT('Origin',(36.,0.,0.));
#9297=CARTESIAN_POINT('Origin',(-0.1,-0.3,-0.82));
#9298=CARTESIAN_POINT('',(0.,-0.3,-1.));
#9299=CARTESIAN_POINT('',(-0.05,-0.3,-1.));
#9300=CARTESIAN_POINT('',(0.,-0.3,-0.82));
#9301=CARTESIAN_POINT('',(0.,-0.3,-0.41));
#9302=CARTESIAN_POINT('',(-0.1,-0.3,-0.82));
#9303=CARTESIAN_POINT('Origin',(0.,-1.,-1.));
#9304=CARTESIAN_POINT('',(0.,-1.,-1.));
#9305=CARTESIAN_POINT('',(0.,-1.,-1.));
#9306=CARTESIAN_POINT('',(0.,-1.,-1.));
#9307=CARTESIAN_POINT('Origin',(0.,-1.,1.));
#9308=CARTESIAN_POINT('',(0.,-1.,-0.3));
#9309=CARTESIAN_POINT('',(-0.05,-1.,-0.3));
#9310=CARTESIAN_POINT('',(0.,-1.,1.));
#9311=CARTESIAN_POINT('Origin',(-0.1,-1.05,-0.3));
#9312=CARTESIAN_POINT('',(0.,-0.82,-0.3));
#9313=CARTESIAN_POINT('',(-0.1,-0.82,-0.3));
#9314=CARTESIAN_POINT('',(0.,-0.525,-0.3));
#9315=CARTESIAN_POINT('Origin',(-0.1,-0.82,-0.3));
#9316=CARTESIAN_POINT('',(0.,-0.82,-0.55));
#9317=CARTESIAN_POINT('',(-0.1,-0.82,-0.55));
#9318=CARTESIAN_POINT('',(0.,-0.82,-0.15));
#9319=CARTESIAN_POINT('Origin',(-0.1,-0.82,-0.55));
#9320=CARTESIAN_POINT('',(0.,-0.67,-0.55));
#9321=CARTESIAN_POINT('',(-0.1,-0.67,-0.55));
#9322=CARTESIAN_POINT('',(0.,-0.41,-0.55));
#9323=CARTESIAN_POINT('Origin',(-0.1,-0.67,-0.55));
#9324=CARTESIAN_POINT('',(0.,-0.42,-0.3));
#9325=CARTESIAN_POINT('',(-0.1,-0.42,-0.3));
#9326=CARTESIAN_POINT('',(0.,-0.365,-0.245));
#9327=CARTESIAN_POINT('Origin',(-0.1,-0.42,-0.3));
#9328=CARTESIAN_POINT('',(0.,-0.42,0.3));
#9329=CARTESIAN_POINT('',(-0.1,-0.42,0.3));
#9330=CARTESIAN_POINT('',(0.,-0.42,-0.15));
#9331=CARTESIAN_POINT('Origin',(-0.1,-0.42,0.3));
#9332=CARTESIAN_POINT('',(0.,-0.67,0.55));
#9333=CARTESIAN_POINT('',(-0.1,-0.67,0.55));
#9334=CARTESIAN_POINT('',(-6.93889390390723E-18,-0.24,0.12));
#9335=CARTESIAN_POINT('Origin',(-0.1,-0.67,0.55));
#9336=CARTESIAN_POINT('',(0.,-0.82,0.55));
#9337=CARTESIAN_POINT('',(-0.1,-0.82,0.55));
#9338=CARTESIAN_POINT('',(0.,-0.335,0.55));
#9339=CARTESIAN_POINT('Origin',(-0.1,-0.82,0.55));
#9340=CARTESIAN_POINT('',(0.,-0.82,0.3));
#9341=CARTESIAN_POINT('',(-0.1,-0.82,0.3));
#9342=CARTESIAN_POINT('',(0.,-0.82,0.275));
#9343=CARTESIAN_POINT('Origin',(-0.1,-0.82,0.3));
#9344=CARTESIAN_POINT('',(0.,-1.,0.3));
#9345=CARTESIAN_POINT('',(-0.05,-1.,0.3));
#9346=CARTESIAN_POINT('',(0.,-0.41,0.3));
#9347=CARTESIAN_POINT('Origin',(0.,-1.,1.));
#9348=CARTESIAN_POINT('',(0.,-1.,1.));
#9349=CARTESIAN_POINT('',(0.,-1.,1.));
#9350=CARTESIAN_POINT('',(0.,-1.,1.));
#9351=CARTESIAN_POINT('Origin',(0.,1.,1.));
#9352=CARTESIAN_POINT('',(0.,-0.3,1.));
#9353=CARTESIAN_POINT('',(-0.05,-0.3,1.));
#9354=CARTESIAN_POINT('',(0.,1.,1.));
#9355=CARTESIAN_POINT('Origin',(-0.1,-0.3,1.05));
#9356=CARTESIAN_POINT('',(0.,-0.3,0.82));
#9357=CARTESIAN_POINT('',(-0.1,-0.3,0.82));
#9358=CARTESIAN_POINT('',(0.,-0.3,0.525));
#9359=CARTESIAN_POINT('Origin',(-0.1,-0.3,0.82));
#9360=CARTESIAN_POINT('',(0.,-0.55,0.82));
#9361=CARTESIAN_POINT('',(-0.1,-0.55,0.82));
#9362=CARTESIAN_POINT('',(0.,-0.15,0.82));
#9363=CARTESIAN_POINT('Origin',(-0.1,-0.55,0.82));
#9364=CARTESIAN_POINT('',(0.,-0.55,0.67));
#9365=CARTESIAN_POINT('',(-0.1,-0.55,0.67));
#9366=CARTESIAN_POINT('',(0.,-0.55,0.41));
#9367=CARTESIAN_POINT('Origin',(-0.1,-0.55,0.67));
#9368=CARTESIAN_POINT('',(0.,-0.3,0.42));
#9369=CARTESIAN_POINT('',(-0.1,-0.3,0.42));
#9370=CARTESIAN_POINT('',(6.93889390390723E-18,-0.245,0.365));
#9371=CARTESIAN_POINT('Origin',(-0.1,-0.3,0.42));
#9372=CARTESIAN_POINT('',(0.,0.3,0.42));
#9373=CARTESIAN_POINT('',(-0.1,0.3,0.42));
#9374=CARTESIAN_POINT('',(0.,-0.15,0.42));
#9375=CARTESIAN_POINT('Origin',(-0.1,0.3,0.42));
#9376=CARTESIAN_POINT('',(0.,0.55,0.67));
#9377=CARTESIAN_POINT('',(-0.1,0.55,0.67));
#9378=CARTESIAN_POINT('',(6.93889390390723E-18,0.12,0.24));
#9379=CARTESIAN_POINT('Origin',(-0.1,0.55,0.67));
#9380=CARTESIAN_POINT('',(0.,0.55,0.82));
#9381=CARTESIAN_POINT('',(-0.1,0.55,0.82));
#9382=CARTESIAN_POINT('',(0.,0.55,0.335));
#9383=CARTESIAN_POINT('Origin',(-0.1,0.55,0.82));
#9384=CARTESIAN_POINT('',(0.,0.3,0.82));
#9385=CARTESIAN_POINT('',(-0.1,0.3,0.82));
#9386=CARTESIAN_POINT('',(0.,0.275,0.82));
#9387=CARTESIAN_POINT('Origin',(-0.1,0.82,-0.3));
#9388=CARTESIAN_POINT('',(0.,1.,-0.3));
#9389=CARTESIAN_POINT('',(-0.05,1.,-0.3));
#9390=CARTESIAN_POINT('',(0.,0.82,-0.3));
#9391=CARTESIAN_POINT('',(0.,0.41,-0.3));
#9392=CARTESIAN_POINT('',(-0.1,0.82,-0.3));
#9393=CARTESIAN_POINT('Origin',(-0.1,0.82,-0.55));
#9394=CARTESIAN_POINT('',(0.,0.82,-0.55));
#9395=CARTESIAN_POINT('',(0.,0.82,-0.275));
#9396=CARTESIAN_POINT('',(-0.1,0.82,-0.55));
#9397=CARTESIAN_POINT('Origin',(-0.1,0.67,-0.55));
#9398=CARTESIAN_POINT('',(0.,0.67,-0.55));
#9399=CARTESIAN_POINT('',(0.,0.335,-0.55));
#9400=CARTESIAN_POINT('',(-0.1,0.67,-0.55));
#9401=CARTESIAN_POINT('Origin',(-0.1,0.42,-0.3));
#9402=CARTESIAN_POINT('',(0.,0.42,-0.3));
#9403=CARTESIAN_POINT('',(0.,0.24,-0.12));
#9404=CARTESIAN_POINT('',(-0.1,0.42,-0.3));
#9405=CARTESIAN_POINT('Origin',(-0.1,0.42,0.3));
#9406=CARTESIAN_POINT('',(0.,0.42,0.3));
#9407=CARTESIAN_POINT('',(0.,0.42,0.15));
#9408=CARTESIAN_POINT('',(-0.1,0.42,0.3));
#9409=CARTESIAN_POINT('Origin',(-0.1,0.67,0.55));
#9410=CARTESIAN_POINT('',(0.,0.67,0.55));
#9411=CARTESIAN_POINT('',(6.93889390390723E-18,0.365,0.245));
#9412=CARTESIAN_POINT('',(-0.1,0.67,0.55));
#9413=CARTESIAN_POINT('Origin',(-0.1,0.82,0.55));
#9414=CARTESIAN_POINT('',(0.,0.82,0.55));
#9415=CARTESIAN_POINT('',(0.,0.41,0.55));
#9416=CARTESIAN_POINT('',(-0.1,0.82,0.55));
#9417=CARTESIAN_POINT('Origin',(-0.1,0.82,0.3));
#9418=CARTESIAN_POINT('',(0.,0.82,0.3));
#9419=CARTESIAN_POINT('',(0.,0.82,0.15));
#9420=CARTESIAN_POINT('',(-0.1,0.82,0.3));
#9421=CARTESIAN_POINT('Origin',(-0.1,1.05,0.3));
#9422=CARTESIAN_POINT('',(0.,1.,0.3));
#9423=CARTESIAN_POINT('',(0.,0.525,0.3));
#9424=CARTESIAN_POINT('',(-0.05,1.,0.3));
#9425=CARTESIAN_POINT('Origin',(-0.1,-0.55,-0.82));
#9426=CARTESIAN_POINT('',(0.,-0.55,-0.82));
#9427=CARTESIAN_POINT('',(0.,-0.275,-0.82));
#9428=CARTESIAN_POINT('',(-0.1,-0.55,-0.82));
#9429=CARTESIAN_POINT('Origin',(-0.1,-0.55,-0.67));
#9430=CARTESIAN_POINT('',(0.,-0.55,-0.67));
#9431=CARTESIAN_POINT('',(0.,-0.55,-0.335));
#9432=CARTESIAN_POINT('',(-0.1,-0.55,-0.67));
#9433=CARTESIAN_POINT('Origin',(-0.1,-0.3,-0.42));
#9434=CARTESIAN_POINT('',(0.,-0.3,-0.42));
#9435=CARTESIAN_POINT('',(0.,-0.12,-0.24));
#9436=CARTESIAN_POINT('',(-0.1,-0.3,-0.42));
#9437=CARTESIAN_POINT('Origin',(-0.1,0.3,-0.42));
#9438=CARTESIAN_POINT('',(0.,0.3,-0.42));
#9439=CARTESIAN_POINT('',(0.,0.15,-0.42));
#9440=CARTESIAN_POINT('',(-0.1,0.3,-0.42));
#9441=CARTESIAN_POINT('Origin',(-0.1,0.55,-0.67));
#9442=CARTESIAN_POINT('',(0.,0.55,-0.67));
#9443=CARTESIAN_POINT('',(0.,0.245,-0.365));
#9444=CARTESIAN_POINT('',(-0.1,0.55,-0.67));
#9445=CARTESIAN_POINT('Origin',(-0.1,0.55,-0.82));
#9446=CARTESIAN_POINT('',(0.,0.55,-0.82));
#9447=CARTESIAN_POINT('',(0.,0.55,-0.41));
#9448=CARTESIAN_POINT('',(-0.1,0.55,-0.82));
#9449=CARTESIAN_POINT('Origin',(-0.1,0.3,-0.82));
#9450=CARTESIAN_POINT('',(0.,0.3,-0.82));
#9451=CARTESIAN_POINT('',(0.,0.15,-0.82));
#9452=CARTESIAN_POINT('',(-0.1,0.3,-0.82));
#9453=CARTESIAN_POINT('Origin',(-0.1,0.3,-1.05));
#9454=CARTESIAN_POINT('',(0.,0.3,-1.));
#9455=CARTESIAN_POINT('',(0.,0.3,-0.525));
#9456=CARTESIAN_POINT('',(-0.05,0.3,-1.));
#9457=CARTESIAN_POINT('Origin',(-0.1,0.3,0.82));
#9458=CARTESIAN_POINT('',(0.,0.3,1.));
#9459=CARTESIAN_POINT('',(-0.05,0.3,1.));
#9460=CARTESIAN_POINT('',(0.,0.3,0.41));
#9461=CARTESIAN_POINT('Origin',(-0.1,0.,0.));
#9462=CARTESIAN_POINT('',(0.,-2.57175827820944E-17,0.21));
#9463=CARTESIAN_POINT('Origin',(0.,0.,0.));
#9464=CARTESIAN_POINT('',(-0.1,-2.57175827820944E-17,0.21));
#9465=CARTESIAN_POINT('Origin',(0.,1.,-1.));
#9466=CARTESIAN_POINT('',(0.,1.,1.));
#9467=CARTESIAN_POINT('',(0.,1.,-1.));
#9468=CARTESIAN_POINT('',(0.,1.,1.));
#9469=CARTESIAN_POINT('Origin',(0.,1.,-1.));
#9470=CARTESIAN_POINT('',(0.,1.,-1.));
#9471=CARTESIAN_POINT('',(0.,1.,-1.));
#9472=CARTESIAN_POINT('',(0.,1.,-1.));
#9473=CARTESIAN_POINT('Origin',(0.,-1.,-1.));
#9474=CARTESIAN_POINT('',(0.,-1.,-1.));
#9475=CARTESIAN_POINT('Origin',(0.,1.,1.));
#9476=CARTESIAN_POINT('',(0.,1.,1.));
#9477=CARTESIAN_POINT('Origin',(0.,0.,0.));
#9478=CARTESIAN_POINT('',(0.,0.,0.));
#9479=CARTESIAN_POINT('Origin',(0.115470053837925,-0.5,-0.2));
#9480=CARTESIAN_POINT('',(0.23094010767585,-0.5,0.));
#9481=CARTESIAN_POINT('',(0.115470053837925,-0.5,-0.2));
#9482=CARTESIAN_POINT('',(0.23094010767585,-0.5,0.));
#9483=CARTESIAN_POINT('',(0.115470053837925,-0.8,-0.2));
#9484=CARTESIAN_POINT('',(0.115470053837925,-0.5,-0.2));
#9485=CARTESIAN_POINT('',(0.23094010767585,-0.8,0.));
#9486=CARTESIAN_POINT('',(0.23094010767585,-0.8,0.));
#9487=CARTESIAN_POINT('',(0.23094010767585,-0.5,0.));
#9488=CARTESIAN_POINT('Origin',(-0.115470053837925,-0.5,-0.2));
#9489=CARTESIAN_POINT('',(-0.115470053837925,-0.5,-0.2));
#9490=CARTESIAN_POINT('',(0.115470053837925,-0.5,-0.2));
#9491=CARTESIAN_POINT('',(-0.115470053837925,-0.8,-0.2));
#9492=CARTESIAN_POINT('',(-0.115470053837925,-0.5,-0.2));
#9493=CARTESIAN_POINT('',(0.115470053837925,-0.8,-0.2));
#9494=CARTESIAN_POINT('Origin',(-0.23094010767585,-0.5,-2.77555756156289E-17));
#9495=CARTESIAN_POINT('',(-0.23094010767585,-0.5,-2.82820063659975E-17));
#9496=CARTESIAN_POINT('',(-0.115470053837925,-0.5,-0.2));
#9497=CARTESIAN_POINT('',(-0.23094010767585,-0.8,-2.77555756156289E-17));
#9498=CARTESIAN_POINT('',(-0.23094010767585,-0.5,-2.82820063659975E-17));
#9499=CARTESIAN_POINT('',(-0.115470053837925,-0.8,-0.2));
#9500=CARTESIAN_POINT('Origin',(-0.115470053837925,-0.5,0.2));
#9501=CARTESIAN_POINT('',(-0.115470053837925,-0.5,0.2));
#9502=CARTESIAN_POINT('',(-0.23094010767585,-0.5,-2.82820063659975E-17));
#9503=CARTESIAN_POINT('',(-0.115470053837925,-0.8,0.2));
#9504=CARTESIAN_POINT('',(-0.115470053837925,-0.5,0.2));
#9505=CARTESIAN_POINT('',(-0.23094010767585,-0.8,-2.82820063659975E-17));
#9506=CARTESIAN_POINT('Origin',(0.115470053837925,-0.5,0.2));
#9507=CARTESIAN_POINT('',(0.115470053837925,-0.5,0.2));
#9508=CARTESIAN_POINT('',(-0.115470053837925,-0.5,0.2));
#9509=CARTESIAN_POINT('',(0.115470053837925,-0.8,0.2));
#9510=CARTESIAN_POINT('',(0.115470053837925,-0.5,0.2));
#9511=CARTESIAN_POINT('',(-0.115470053837925,-0.8,0.2));
#9512=CARTESIAN_POINT('Origin',(0.23094010767585,-0.5,0.));
#9513=CARTESIAN_POINT('',(0.115470053837925,-0.5,0.2));
#9514=CARTESIAN_POINT('',(0.115470053837925,-0.8,0.2));
#9515=CARTESIAN_POINT('Origin',(0.,-0.5,0.));
#9516=CARTESIAN_POINT('Origin',(0.,-0.8,0.));
#9517=CARTESIAN_POINT('Origin',(0.,-1.9,0.));
#9518=CARTESIAN_POINT('',(-0.25,-1.9,3.06161699786838E-17));
#9519=CARTESIAN_POINT('Origin',(0.,-1.9,0.));
#9520=CARTESIAN_POINT('',(-0.24505,-1.9,3.00099698131059E-17));
#9521=CARTESIAN_POINT('Origin',(0.,-1.9,0.));
#9522=CARTESIAN_POINT('Origin',(0.,-3.,0.));
#9523=CARTESIAN_POINT('',(-0.25,-3.,3.06161699786838E-17));
#9524=CARTESIAN_POINT('',(-0.25,-3.,3.06161699786838E-17));
#9525=CARTESIAN_POINT('Origin',(0.,-3.,0.));
#9526=CARTESIAN_POINT('Origin',(0.,-3.,0.));
#9527=CARTESIAN_POINT('Origin',(0.375,0.5,0.));
#9528=CARTESIAN_POINT('',(-0.375,0.5,-4.59242549680257E-17));
#9529=CARTESIAN_POINT('Origin',(0.,0.5,0.));
#9530=CARTESIAN_POINT('Origin',(0.,0.475,0.));
#9531=CARTESIAN_POINT('',(-0.425,0.45,-5.20474889637625E-17));
#9532=CARTESIAN_POINT('Origin',(0.,0.45,0.));
#9533=CARTESIAN_POINT('',(-0.4,0.475,-4.89858719658941E-17));
#9534=CARTESIAN_POINT('Origin',(0.,0.24,0.));
#9535=CARTESIAN_POINT('',(-0.425,0.0299999999999998,-5.20474889637625E-17));
#9536=CARTESIAN_POINT('Origin',(0.,0.0299999999999998,0.));
#9537=CARTESIAN_POINT('',(-0.425,0.24,-5.20474889637625E-17));
#9538=CARTESIAN_POINT('Origin',(0.,0.0150000000000001,0.));
#9539=CARTESIAN_POINT('',(-0.395,4.85722573273506E-17,-4.83735485663204E-17));
#9540=CARTESIAN_POINT('Origin',(0.,0.,0.));
#9541=CARTESIAN_POINT('',(-0.41,0.0150000000000001,-5.02105187650415E-17));
#9542=CARTESIAN_POINT('Origin',(0.27,0.,0.));
#9543=CARTESIAN_POINT('',(-0.27,0.,-3.30654635769785E-17));
#9544=CARTESIAN_POINT('Origin',(0.,0.,0.));
#9545=CARTESIAN_POINT('Origin',(0.,-0.02,0.));
#9546=CARTESIAN_POINT('',(-0.24505,-0.0498999999999999,3.00099698131059E-17));
#9547=CARTESIAN_POINT('Origin',(0.,-0.0498999999999999,0.));
#9548=CARTESIAN_POINT('',(-0.26,-0.02,-3.18408167778312E-17));
#9549=CARTESIAN_POINT('Origin',(0.,-0.995,0.));
#9550=CARTESIAN_POINT('',(-0.24505,-0.995,-3.00099698131059E-17));
#9551=CARTESIAN_POINT('',(0.,0.,0.));
#9552=CARTESIAN_POINT('Origin',(0.375,0.5,0.));
#9553=CARTESIAN_POINT('',(-0.375,0.5,-4.59242549680257E-17));
#9554=CARTESIAN_POINT('Origin',(0.,0.5,0.));
#9555=CARTESIAN_POINT('Origin',(0.,0.475,0.));
#9556=CARTESIAN_POINT('',(-0.425,0.45,-5.20474889637625E-17));
#9557=CARTESIAN_POINT('Origin',(0.,0.45,0.));
#9558=CARTESIAN_POINT('',(-0.4,0.475,-4.89858719658941E-17));
#9559=CARTESIAN_POINT('Origin',(0.,0.24,0.));
#9560=CARTESIAN_POINT('',(-0.425,0.0299999999999998,-5.20474889637625E-17));
#9561=CARTESIAN_POINT('Origin',(0.,0.0299999999999998,0.));
#9562=CARTESIAN_POINT('',(-0.425,0.24,-5.20474889637625E-17));
#9563=CARTESIAN_POINT('Origin',(0.,0.0150000000000001,0.));
#9564=CARTESIAN_POINT('',(-0.395,4.85722573273506E-17,-4.83735485663204E-17));
#9565=CARTESIAN_POINT('Origin',(0.,0.,0.));
#9566=CARTESIAN_POINT('',(-0.41,0.0150000000000001,-5.02105187650415E-17));
#9567=CARTESIAN_POINT('Origin',(0.27,0.,0.));
#9568=CARTESIAN_POINT('',(-0.27,0.,-3.30654635769785E-17));
#9569=CARTESIAN_POINT('Origin',(0.,0.,0.));
#9570=CARTESIAN_POINT('Origin',(0.,-0.02,0.));
#9571=CARTESIAN_POINT('',(-0.24505,-0.0498999999999999,3.00099698131059E-17));
#9572=CARTESIAN_POINT('Origin',(0.,-0.0498999999999999,0.));
#9573=CARTESIAN_POINT('',(-0.26,-0.02,-3.18408167778312E-17));
#9574=CARTESIAN_POINT('Origin',(0.,-0.995,0.));
#9575=CARTESIAN_POINT('',(-0.24505,-1.95495,3.00099698131059E-17));
#9576=CARTESIAN_POINT('Origin',(0.,-1.95495,0.));
#9577=CARTESIAN_POINT('',(-0.24505,-0.995,-3.00099698131059E-17));
#9578=CARTESIAN_POINT('Origin',(0.,-1.975,0.));
#9579=CARTESIAN_POINT('',(-0.2,-2.,-2.44929359829471E-17));
#9580=CARTESIAN_POINT('Origin',(0.,-2.,0.));
#9581=CARTESIAN_POINT('',(-0.225,-1.975,-2.75545529808154E-17));
#9582=CARTESIAN_POINT('Origin',(0.,-2.,0.));
#9583=CARTESIAN_POINT('Origin',(0.115470053837925,-0.5,-0.2));
#9584=CARTESIAN_POINT('',(0.23094010767585,-0.5,0.));
#9585=CARTESIAN_POINT('',(0.115470053837925,-0.5,-0.2));
#9586=CARTESIAN_POINT('',(0.23094010767585,-0.5,0.));
#9587=CARTESIAN_POINT('',(0.115470053837925,-0.8,-0.2));
#9588=CARTESIAN_POINT('',(0.115470053837925,-0.5,-0.2));
#9589=CARTESIAN_POINT('',(0.23094010767585,-0.8,0.));
#9590=CARTESIAN_POINT('',(0.23094010767585,-0.8,0.));
#9591=CARTESIAN_POINT('',(0.23094010767585,-0.5,0.));
#9592=CARTESIAN_POINT('Origin',(-0.115470053837925,-0.5,-0.2));
#9593=CARTESIAN_POINT('',(-0.115470053837925,-0.5,-0.2));
#9594=CARTESIAN_POINT('',(0.115470053837925,-0.5,-0.2));
#9595=CARTESIAN_POINT('',(-0.115470053837925,-0.8,-0.2));
#9596=CARTESIAN_POINT('',(-0.115470053837925,-0.5,-0.2));
#9597=CARTESIAN_POINT('',(0.115470053837925,-0.8,-0.2));
#9598=CARTESIAN_POINT('Origin',(-0.23094010767585,-0.5,-2.77555756156289E-17));
#9599=CARTESIAN_POINT('',(-0.23094010767585,-0.5,-2.82820063659975E-17));
#9600=CARTESIAN_POINT('',(-0.115470053837925,-0.5,-0.2));
#9601=CARTESIAN_POINT('',(-0.23094010767585,-0.8,-2.77555756156289E-17));
#9602=CARTESIAN_POINT('',(-0.23094010767585,-0.5,-2.82820063659975E-17));
#9603=CARTESIAN_POINT('',(-0.115470053837925,-0.8,-0.2));
#9604=CARTESIAN_POINT('Origin',(-0.115470053837925,-0.5,0.2));
#9605=CARTESIAN_POINT('',(-0.115470053837925,-0.5,0.2));
#9606=CARTESIAN_POINT('',(-0.23094010767585,-0.5,-2.82820063659975E-17));
#9607=CARTESIAN_POINT('',(-0.115470053837925,-0.8,0.2));
#9608=CARTESIAN_POINT('',(-0.115470053837925,-0.5,0.2));
#9609=CARTESIAN_POINT('',(-0.23094010767585,-0.8,-2.82820063659975E-17));
#9610=CARTESIAN_POINT('Origin',(0.115470053837925,-0.5,0.2));
#9611=CARTESIAN_POINT('',(0.115470053837925,-0.5,0.2));
#9612=CARTESIAN_POINT('',(-0.115470053837925,-0.5,0.2));
#9613=CARTESIAN_POINT('',(0.115470053837925,-0.8,0.2));
#9614=CARTESIAN_POINT('',(0.115470053837925,-0.5,0.2));
#9615=CARTESIAN_POINT('',(-0.115470053837925,-0.8,0.2));
#9616=CARTESIAN_POINT('Origin',(0.23094010767585,-0.5,0.));
#9617=CARTESIAN_POINT('',(0.115470053837925,-0.5,0.2));
#9618=CARTESIAN_POINT('',(0.115470053837925,-0.8,0.2));
#9619=CARTESIAN_POINT('Origin',(0.,-0.5,0.));
#9620=CARTESIAN_POINT('Origin',(0.,-0.8,0.));
#9621=CARTESIAN_POINT('',(0.,0.,0.));
#9622=CARTESIAN_POINT('Origin',(0.,0.395,0.25));
#9623=CARTESIAN_POINT('',(-0.5,0.3,0.25));
#9624=CARTESIAN_POINT('',(0.5,0.3,0.25));
#9625=CARTESIAN_POINT('',(0.25,0.3,0.25));
#9626=CARTESIAN_POINT('',(-0.5,0.5,0.25));
#9627=CARTESIAN_POINT('',(-0.5,0.5,0.25));
#9628=CARTESIAN_POINT('',(0.5,0.5,0.25));
#9629=CARTESIAN_POINT('',(0.5,0.5,0.25));
#9630=CARTESIAN_POINT('',(0.5,0.29,0.25));
#9631=CARTESIAN_POINT('Origin',(0.5,0.5,0.25));
#9632=CARTESIAN_POINT('',(-0.5,0.5,0.4));
#9633=CARTESIAN_POINT('',(-0.5,0.5,0.25));
#9634=CARTESIAN_POINT('',(0.5,0.5,0.4));
#9635=CARTESIAN_POINT('',(0.5,0.5,0.4));
#9636=CARTESIAN_POINT('',(0.5,0.5,0.25));
#9637=CARTESIAN_POINT('Origin',(0.,0.,0.4));
#9638=CARTESIAN_POINT('',(-0.5,-0.5,0.4));
#9639=CARTESIAN_POINT('',(-0.5,0.5,0.4));
#9640=CARTESIAN_POINT('',(0.5,-0.5,0.4));
#9641=CARTESIAN_POINT('',(-0.5,-0.5,0.4));
#9642=CARTESIAN_POINT('',(0.5,-0.3,0.4));
#9643=CARTESIAN_POINT('',(-0.2117,2.59257727379495E-17,0.4));
#9644=CARTESIAN_POINT('Origin',(0.,0.,0.4));
#9645=CARTESIAN_POINT('Origin',(-0.5,0.3,0.));
#9646=CARTESIAN_POINT('',(-0.5,0.3,0.15));
#9647=CARTESIAN_POINT('',(-0.5,0.3,0.));
#9648=CARTESIAN_POINT('',(-0.5,0.15,0.));
#9649=CARTESIAN_POINT('',(-0.5,0.225,0.075));
#9650=CARTESIAN_POINT('',(-0.5,-0.15,0.));
#9651=CARTESIAN_POINT('',(-0.5,0.3,0.));
#9652=CARTESIAN_POINT('',(-0.5,-0.3,0.15));
#9653=CARTESIAN_POINT('',(-0.5,-0.075,-0.075));
#9654=CARTESIAN_POINT('',(-0.5,-0.3,0.25));
#9655=CARTESIAN_POINT('',(-0.5,-0.3,0.));
#9656=CARTESIAN_POINT('',(-0.5,-0.5,0.25));
#9657=CARTESIAN_POINT('',(-0.5,-0.29,0.25));
#9658=CARTESIAN_POINT('',(-0.5,-0.5,0.25));
#9659=CARTESIAN_POINT('Origin',(-0.5,-0.5,0.25));
#9660=CARTESIAN_POINT('',(0.5,-0.5,0.25));
#9661=CARTESIAN_POINT('',(-0.5,-0.5,0.25));
#9662=CARTESIAN_POINT('',(0.5,-0.5,0.25));
#9663=CARTESIAN_POINT('Origin',(0.,-0.395,0.25));
#9664=CARTESIAN_POINT('',(0.5,-0.3,0.25));
#9665=CARTESIAN_POINT('',(-0.25,-0.3,0.25));
#9666=CARTESIAN_POINT('',(0.5,-0.5,0.25));
#9667=CARTESIAN_POINT('Origin',(0.5,-0.3,0.));
#9668=CARTESIAN_POINT('',(0.5,-0.3,0.15));
#9669=CARTESIAN_POINT('',(0.5,-0.3,0.));
#9670=CARTESIAN_POINT('',(0.5,-0.15,0.));
#9671=CARTESIAN_POINT('',(0.5,-0.225,0.075));
#9672=CARTESIAN_POINT('',(0.5,0.15,0.));
#9673=CARTESIAN_POINT('',(0.5,-0.3,0.));
#9674=CARTESIAN_POINT('',(0.5,0.3,0.15));
#9675=CARTESIAN_POINT('',(0.5,0.075,-0.075));
#9676=CARTESIAN_POINT('',(0.5,0.3,0.));
#9677=CARTESIAN_POINT('Origin',(-0.5,-0.3,0.));
#9678=CARTESIAN_POINT('',(-0.25,-0.3,0.15));
#9679=CARTESIAN_POINT('Origin',(-0.25,-0.225,0.075));
#9680=CARTESIAN_POINT('',(-0.149388386429468,-0.15,0.));
#9681=CARTESIAN_POINT('',(-0.25,-0.15,0.));
#9682=CARTESIAN_POINT('',(0.149388386429468,-0.15,0.));
#9683=CARTESIAN_POINT('Origin',(0.,0.,-0.15));
#9684=CARTESIAN_POINT('',(-0.25,-0.15,0.));
#9685=CARTESIAN_POINT('Origin',(0.,0.,-0.1));
#9686=CARTESIAN_POINT('',(-0.2117,-2.59257727379495E-17,0.));
#9687=CARTESIAN_POINT('Origin',(0.,0.,0.));
#9688=CARTESIAN_POINT('',(-0.2117,-2.59257727379495E-17,-0.1));
#9689=CARTESIAN_POINT('',(-0.149388386429468,0.15,0.));
#9690=CARTESIAN_POINT('Origin',(0.,0.,0.));
#9691=CARTESIAN_POINT('',(0.149388386429468,0.15,0.));
#9692=CARTESIAN_POINT('Origin',(0.,0.,-0.15));
#9693=CARTESIAN_POINT('Origin',(0.,0.,0.));
#9694=CARTESIAN_POINT('Origin',(0.,0.,0.));
#9695=CARTESIAN_POINT('',(0.25,0.15,0.));
#9696=CARTESIAN_POINT('Origin',(0.,0.,0.));
#9697=CARTESIAN_POINT('',(0.25,0.15,0.));
#9698=CARTESIAN_POINT('Origin',(0.25,0.225,0.075));
#9699=CARTESIAN_POINT('',(0.25,0.3,0.15));
#9700=CARTESIAN_POINT('Origin',(0.5,0.3,0.));
#9701=CARTESIAN_POINT('',(0.,0.,0.));
#9702=CARTESIAN_POINT('Origin',(0.,0.09,0.));
#9703=CARTESIAN_POINT('',(-0.285,0.1,3.49024337756996E-17));
#9704=CARTESIAN_POINT('Origin',(0.,0.1,0.));
#9705=CARTESIAN_POINT('',(-0.265,0.08,-3.24531401774049E-17));
#9706=CARTESIAN_POINT('',(-0.275,0.09,3.36777869765522E-17));
#9707=CARTESIAN_POINT('Origin',(0.,0.08,0.));
#9708=CARTESIAN_POINT('Origin',(0.,0.,0.));
#9709=CARTESIAN_POINT('',(-0.265,0.,3.24531401774049E-17));
#9710=CARTESIAN_POINT('',(-0.265,0.,3.24531401774049E-17));
#9711=CARTESIAN_POINT('Origin',(0.,0.,0.));
#9712=CARTESIAN_POINT('Origin',(0.,0.1,0.));
#9713=CARTESIAN_POINT('',(-0.5,0.1,6.12323399573677E-17));
#9714=CARTESIAN_POINT('Origin',(0.,0.1,0.));
#9715=CARTESIAN_POINT('Origin',(0.,0.,0.));
#9716=CARTESIAN_POINT('',(-0.5,0.,6.12323399573677E-17));
#9717=CARTESIAN_POINT('',(-0.5,0.,6.12323399573677E-17));
#9718=CARTESIAN_POINT('Origin',(0.,0.,0.));
#9719=CARTESIAN_POINT('Origin',(0.,0.,0.));
#9720=CARTESIAN_POINT('',(0.,0.,0.));
#9721=CARTESIAN_POINT('Origin',(0.115470053837925,-0.5,-0.2));
#9722=CARTESIAN_POINT('',(0.23094010767585,-0.5,0.));
#9723=CARTESIAN_POINT('',(0.115470053837925,-0.5,-0.2));
#9724=CARTESIAN_POINT('',(0.23094010767585,-0.5,0.));
#9725=CARTESIAN_POINT('',(0.115470053837925,-0.8,-0.2));
#9726=CARTESIAN_POINT('',(0.115470053837925,-0.5,-0.2));
#9727=CARTESIAN_POINT('',(0.23094010767585,-0.8,0.));
#9728=CARTESIAN_POINT('',(0.23094010767585,-0.8,0.));
#9729=CARTESIAN_POINT('',(0.23094010767585,-0.5,0.));
#9730=CARTESIAN_POINT('Origin',(-0.115470053837925,-0.5,-0.2));
#9731=CARTESIAN_POINT('',(-0.115470053837925,-0.5,-0.2));
#9732=CARTESIAN_POINT('',(0.115470053837925,-0.5,-0.2));
#9733=CARTESIAN_POINT('',(-0.115470053837925,-0.8,-0.2));
#9734=CARTESIAN_POINT('',(-0.115470053837925,-0.5,-0.2));
#9735=CARTESIAN_POINT('',(0.115470053837925,-0.8,-0.2));
#9736=CARTESIAN_POINT('Origin',(-0.23094010767585,-0.5,-2.77555756156289E-17));
#9737=CARTESIAN_POINT('',(-0.23094010767585,-0.5,-2.82820063659975E-17));
#9738=CARTESIAN_POINT('',(-0.115470053837925,-0.5,-0.2));
#9739=CARTESIAN_POINT('',(-0.23094010767585,-0.8,-2.77555756156289E-17));
#9740=CARTESIAN_POINT('',(-0.23094010767585,-0.5,-2.82820063659975E-17));
#9741=CARTESIAN_POINT('',(-0.115470053837925,-0.8,-0.2));
#9742=CARTESIAN_POINT('Origin',(-0.115470053837925,-0.5,0.2));
#9743=CARTESIAN_POINT('',(-0.115470053837925,-0.5,0.2));
#9744=CARTESIAN_POINT('',(-0.23094010767585,-0.5,-2.82820063659975E-17));
#9745=CARTESIAN_POINT('',(-0.115470053837925,-0.8,0.2));
#9746=CARTESIAN_POINT('',(-0.115470053837925,-0.5,0.2));
#9747=CARTESIAN_POINT('',(-0.23094010767585,-0.8,-2.82820063659975E-17));
#9748=CARTESIAN_POINT('Origin',(0.115470053837925,-0.5,0.2));
#9749=CARTESIAN_POINT('',(0.115470053837925,-0.5,0.2));
#9750=CARTESIAN_POINT('',(-0.115470053837925,-0.5,0.2));
#9751=CARTESIAN_POINT('',(0.115470053837925,-0.8,0.2));
#9752=CARTESIAN_POINT('',(0.115470053837925,-0.5,0.2));
#9753=CARTESIAN_POINT('',(-0.115470053837925,-0.8,0.2));
#9754=CARTESIAN_POINT('Origin',(0.23094010767585,-0.5,0.));
#9755=CARTESIAN_POINT('',(0.115470053837925,-0.5,0.2));
#9756=CARTESIAN_POINT('',(0.115470053837925,-0.8,0.2));
#9757=CARTESIAN_POINT('Origin',(0.,-0.5,0.));
#9758=CARTESIAN_POINT('Origin',(0.,-0.8,0.));
#9759=CARTESIAN_POINT('Origin',(0.,-1.4,0.));
#9760=CARTESIAN_POINT('',(-0.24505,-1.4,3.00099698131059E-17));
#9761=CARTESIAN_POINT('Origin',(0.,-1.4,0.));
#9762=CARTESIAN_POINT('Origin',(0.375,0.5,0.));
#9763=CARTESIAN_POINT('',(-0.375,0.5,-4.59242549680257E-17));
#9764=CARTESIAN_POINT('Origin',(0.,0.5,0.));
#9765=CARTESIAN_POINT('Origin',(0.,0.475,0.));
#9766=CARTESIAN_POINT('',(-0.425,0.45,-5.20474889637625E-17));
#9767=CARTESIAN_POINT('Origin',(0.,0.45,0.));
#9768=CARTESIAN_POINT('',(-0.4,0.475,-4.89858719658941E-17));
#9769=CARTESIAN_POINT('Origin',(0.,0.24,0.));
#9770=CARTESIAN_POINT('',(-0.425,0.0299999999999998,-5.20474889637625E-17));
#9771=CARTESIAN_POINT('Origin',(0.,0.0299999999999998,0.));
#9772=CARTESIAN_POINT('',(-0.425,0.24,-5.20474889637625E-17));
#9773=CARTESIAN_POINT('Origin',(0.,0.0150000000000001,0.));
#9774=CARTESIAN_POINT('',(-0.395,4.85722573273506E-17,-4.83735485663204E-17));
#9775=CARTESIAN_POINT('Origin',(0.,0.,0.));
#9776=CARTESIAN_POINT('',(-0.41,0.0150000000000001,-5.02105187650415E-17));
#9777=CARTESIAN_POINT('Origin',(0.27,0.,0.));
#9778=CARTESIAN_POINT('',(-0.27,0.,-3.30654635769785E-17));
#9779=CARTESIAN_POINT('Origin',(0.,0.,0.));
#9780=CARTESIAN_POINT('Origin',(0.,-0.02,0.));
#9781=CARTESIAN_POINT('',(-0.24505,-0.0498999999999999,3.00099698131059E-17));
#9782=CARTESIAN_POINT('Origin',(0.,-0.0498999999999999,0.));
#9783=CARTESIAN_POINT('',(-0.26,-0.02,-3.18408167778312E-17));
#9784=CARTESIAN_POINT('Origin',(0.,-0.995,0.));
#9785=CARTESIAN_POINT('',(-0.24505,-0.995,-3.00099698131059E-17));
#9786=CARTESIAN_POINT('',(0.,0.,0.));
#9787=CARTESIAN_POINT('Origin',(0.,0.07,0.));
#9788=CARTESIAN_POINT('',(-0.235,0.08,2.87791997799628E-17));
#9789=CARTESIAN_POINT('Origin',(0.,0.08,0.));
#9790=CARTESIAN_POINT('',(-0.215,0.06,-2.63299061816681E-17));
#9791=CARTESIAN_POINT('',(-0.225,0.07,2.75545529808154E-17));
#9792=CARTESIAN_POINT('Origin',(0.,0.06,0.));
#9793=CARTESIAN_POINT('Origin',(0.,0.,0.));
#9794=CARTESIAN_POINT('',(-0.215,0.,2.63299061816681E-17));
#9795=CARTESIAN_POINT('',(-0.215,0.,2.63299061816681E-17));
#9796=CARTESIAN_POINT('Origin',(0.,0.,0.));
#9797=CARTESIAN_POINT('Origin',(0.,0.08,0.));
#9798=CARTESIAN_POINT('',(-0.45,0.08,5.51091059616309E-17));
#9799=CARTESIAN_POINT('Origin',(0.,0.08,0.));
#9800=CARTESIAN_POINT('Origin',(0.,0.,0.));
#9801=CARTESIAN_POINT('',(-0.45,0.,5.51091059616309E-17));
#9802=CARTESIAN_POINT('',(-0.45,0.,5.51091059616309E-17));
#9803=CARTESIAN_POINT('Origin',(0.,0.,0.));
#9804=CARTESIAN_POINT('Origin',(0.,0.,0.));
#9805=CARTESIAN_POINT('',(0.,0.,0.));
#9806=CARTESIAN_POINT('Origin',(0.3,0.4,0.));
#9807=CARTESIAN_POINT('',(-0.3,0.4,-3.67394039744206E-17));
#9808=CARTESIAN_POINT('Origin',(0.,0.4,0.));
#9809=CARTESIAN_POINT('Origin',(0.,0.375,0.));
#9810=CARTESIAN_POINT('',(-0.35,0.35,-4.28626379701573E-17));
#9811=CARTESIAN_POINT('Origin',(0.,0.35,0.));
#9812=CARTESIAN_POINT('',(-0.325,0.375,-3.9801020972289E-17));
#9813=CARTESIAN_POINT('Origin',(0.,0.19,0.));
#9814=CARTESIAN_POINT('',(-0.35,0.03,-4.28626379701574E-17));
#9815=CARTESIAN_POINT('Origin',(0.,0.03,0.));
#9816=CARTESIAN_POINT('',(-0.35,0.19,-4.28626379701574E-17));
#9817=CARTESIAN_POINT('Origin',(0.,0.0149999999999999,0.));
#9818=CARTESIAN_POINT('',(-0.32,-3.29597460435593E-17,-3.91886975727153E-17));
#9819=CARTESIAN_POINT('Origin',(0.,0.,0.));
#9820=CARTESIAN_POINT('',(-0.335,0.0149999999999999,-4.10256677714363E-17));
#9821=CARTESIAN_POINT('Origin',(0.22,0.,0.));
#9822=CARTESIAN_POINT('',(-0.22,-6.93889390390723E-18,-2.69422295812418E-17));
#9823=CARTESIAN_POINT('Origin',(0.,0.,0.));
#9824=CARTESIAN_POINT('Origin',(0.,-0.02,0.));
#9825=CARTESIAN_POINT('',(-0.1954,-0.0492,2.39295984553393E-17));
#9826=CARTESIAN_POINT('Origin',(0.,-0.0492,0.));
#9827=CARTESIAN_POINT('',(-0.21,-0.02,-2.57175827820944E-17));
#9828=CARTESIAN_POINT('Origin',(0.,-0.8,0.));
#9829=CARTESIAN_POINT('',(-0.1954,-1.5646,2.39295984553393E-17));
#9830=CARTESIAN_POINT('Origin',(0.,-1.5646,0.));
#9831=CARTESIAN_POINT('',(-0.1954,-0.8,-2.39295984553393E-17));
#9832=CARTESIAN_POINT('Origin',(0.,-1.58,0.));
#9833=CARTESIAN_POINT('',(-0.16,-1.6,-1.95943487863577E-17));
#9834=CARTESIAN_POINT('Origin',(0.,-1.6,0.));
#9835=CARTESIAN_POINT('',(-0.18,-1.58,-2.20436423846524E-17));
#9836=CARTESIAN_POINT('Origin',(0.,-1.6,0.));
#9837=CARTESIAN_POINT('Origin',(0.0866025403784439,-0.4,-0.15));
#9838=CARTESIAN_POINT('',(0.173205080756888,-0.4,0.));
#9839=CARTESIAN_POINT('',(0.0866025403784439,-0.4,-0.15));
#9840=CARTESIAN_POINT('',(0.173205080756888,-0.4,0.));
#9841=CARTESIAN_POINT('',(0.0866025403784439,-0.64,-0.15));
#9842=CARTESIAN_POINT('',(0.0866025403784439,-0.4,-0.15));
#9843=CARTESIAN_POINT('',(0.173205080756888,-0.64,0.));
#9844=CARTESIAN_POINT('',(0.173205080756888,-0.64,0.));
#9845=CARTESIAN_POINT('',(0.173205080756888,-0.4,0.));
#9846=CARTESIAN_POINT('Origin',(-0.0866025403784438,-0.4,-0.15));
#9847=CARTESIAN_POINT('',(-0.0866025403784438,-0.4,-0.15));
#9848=CARTESIAN_POINT('',(0.0866025403784439,-0.4,-0.15));
#9849=CARTESIAN_POINT('',(-0.0866025403784438,-0.64,-0.15));
#9850=CARTESIAN_POINT('',(-0.0866025403784438,-0.4,-0.15));
#9851=CARTESIAN_POINT('',(0.0866025403784439,-0.64,-0.15));
#9852=CARTESIAN_POINT('Origin',(-0.173205080756888,-0.4,-2.77555756156289E-17));
#9853=CARTESIAN_POINT('',(-0.173205080756888,-0.4,-2.12115047744981E-17));
#9854=CARTESIAN_POINT('',(-0.0866025403784438,-0.4,-0.15));
#9855=CARTESIAN_POINT('',(-0.173205080756888,-0.64,-2.77555756156289E-17));
#9856=CARTESIAN_POINT('',(-0.173205080756888,-0.4,-2.12115047744981E-17));
#9857=CARTESIAN_POINT('',(-0.0866025403784438,-0.64,-0.15));
#9858=CARTESIAN_POINT('Origin',(-0.0866025403784439,-0.4,0.15));
#9859=CARTESIAN_POINT('',(-0.0866025403784439,-0.4,0.15));
#9860=CARTESIAN_POINT('',(-0.173205080756888,-0.4,-2.12115047744981E-17));
#9861=CARTESIAN_POINT('',(-0.0866025403784439,-0.64,0.15));
#9862=CARTESIAN_POINT('',(-0.0866025403784439,-0.4,0.15));
#9863=CARTESIAN_POINT('',(-0.173205080756888,-0.64,-2.12115047744981E-17));
#9864=CARTESIAN_POINT('Origin',(0.0866025403784439,-0.4,0.15));
#9865=CARTESIAN_POINT('',(0.0866025403784439,-0.4,0.15));
#9866=CARTESIAN_POINT('',(-0.0866025403784439,-0.4,0.15));
#9867=CARTESIAN_POINT('',(0.0866025403784439,-0.64,0.15));
#9868=CARTESIAN_POINT('',(0.0866025403784439,-0.4,0.15));
#9869=CARTESIAN_POINT('',(-0.0866025403784439,-0.64,0.15));
#9870=CARTESIAN_POINT('Origin',(0.173205080756888,-0.4,0.));
#9871=CARTESIAN_POINT('',(0.0866025403784439,-0.4,0.15));
#9872=CARTESIAN_POINT('',(0.0866025403784439,-0.64,0.15));
#9873=CARTESIAN_POINT('Origin',(0.,-0.4,-2.77555756156289E-17));
#9874=CARTESIAN_POINT('Origin',(0.,-0.64,-2.77555756156289E-17));
#9875=CARTESIAN_POINT('',(0.,0.,0.));
#9876=CARTESIAN_POINT('',(0.,0.,0.));
#9877=CARTESIAN_POINT('',(0.,0.,0.));
#9878=CARTESIAN_POINT('',(0.,0.,0.));
#9879=CARTESIAN_POINT('',(0.,0.,0.));
#9880=CARTESIAN_POINT('',(0.,0.,0.));
#9881=CARTESIAN_POINT('',(0.,0.,0.));
#9882=CARTESIAN_POINT('',(0.,0.,0.));
#9883=CARTESIAN_POINT('',(0.,0.,0.));
#9884=CARTESIAN_POINT('',(0.,0.,0.));
#9885=CARTESIAN_POINT('',(0.,0.,0.));
#9886=CARTESIAN_POINT('',(0.,0.,0.));
#9887=CARTESIAN_POINT('',(0.,0.,0.));
#9888=CARTESIAN_POINT('',(-19.,-19.,0.));
#9889=CARTESIAN_POINT('',(-19.,-19.,-0.8));
#9890=CARTESIAN_POINT('',(-19.,-19.,-0.9));
#9891=CARTESIAN_POINT('',(-19.,19.,0.));
#9892=CARTESIAN_POINT('',(-19.,19.,-0.8));
#9893=CARTESIAN_POINT('',(-19.,19.,-0.9));
#9894=CARTESIAN_POINT('',(19.,-19.,0.));
#9895=CARTESIAN_POINT('',(19.,-19.,-0.8));
#9896=CARTESIAN_POINT('',(19.,-19.,-0.9));
#9897=CARTESIAN_POINT('',(19.,19.,0.));
#9898=CARTESIAN_POINT('',(19.,19.,-0.8));
#9899=CARTESIAN_POINT('',(19.,19.,-0.9));
#9900=CARTESIAN_POINT('',(-18.,-19.,1.));
#9901=CARTESIAN_POINT('',(-20.,-19.,1.));
#9902=CARTESIAN_POINT('',(-20.1,-19.,1.));
#9903=CARTESIAN_POINT('',(20.,-19.,1.));
#9904=CARTESIAN_POINT('',(20.1,-19.,1.));
#9905=CARTESIAN_POINT('',(-18.,-19.,37.));
#9906=CARTESIAN_POINT('',(-20.,-19.,37.));
#9907=CARTESIAN_POINT('',(-20.1,-19.,37.));
#9908=CARTESIAN_POINT('',(20.,-19.,37.));
#9909=CARTESIAN_POINT('',(20.1,-19.,37.));
#9910=CARTESIAN_POINT('',(-18.,19.,1.));
#9911=CARTESIAN_POINT('',(-20.,19.,1.));
#9912=CARTESIAN_POINT('',(-20.1,19.,1.));
#9913=CARTESIAN_POINT('',(20.,19.,1.));
#9914=CARTESIAN_POINT('',(20.1,19.,1.));
#9915=CARTESIAN_POINT('',(-18.,19.,37.));
#9916=CARTESIAN_POINT('',(-20.,19.,37.));
#9917=CARTESIAN_POINT('',(-20.1,19.,37.));
#9918=CARTESIAN_POINT('',(20.,19.,37.));
#9919=CARTESIAN_POINT('',(20.1,19.,37.));
#9920=CARTESIAN_POINT('',(-19.,-18.,4.));
#9921=CARTESIAN_POINT('',(-19.,-20.,4.));
#9922=CARTESIAN_POINT('',(-19.,-20.1,4.));
#9923=CARTESIAN_POINT('',(-19.,20.,4.));
#9924=CARTESIAN_POINT('',(-19.,20.1,4.));
#9925=CARTESIAN_POINT('',(-19.,-18.,34.));
#9926=CARTESIAN_POINT('',(-19.,-20.,34.));
#9927=CARTESIAN_POINT('',(-19.,-20.1,34.));
#9928=CARTESIAN_POINT('',(-19.,20.,34.));
#9929=CARTESIAN_POINT('',(-19.,20.1,34.));
#9930=CARTESIAN_POINT('',(19.,-18.,4.));
#9931=CARTESIAN_POINT('',(19.,-20.,4.));
#9932=CARTESIAN_POINT('',(19.,-20.1,4.));
#9933=CARTESIAN_POINT('',(19.,20.,4.));
#9934=CARTESIAN_POINT('',(19.,20.1,4.));
#9935=CARTESIAN_POINT('',(19.,-18.,34.));
#9936=CARTESIAN_POINT('',(19.,-20.,34.));
#9937=CARTESIAN_POINT('',(19.,-20.1,34.));
#9938=CARTESIAN_POINT('',(19.,20.,34.));
#9939=CARTESIAN_POINT('',(19.,20.1,34.));
#9940=CARTESIAN_POINT('',(-19.,-19.,40.7));
#9941=CARTESIAN_POINT('',(-19.,19.,40.7));
#9942=CARTESIAN_POINT('',(19.,-19.,40.7));
#9943=CARTESIAN_POINT('',(19.,19.,40.7));
#9944=CARTESIAN_POINT('',(-19.,-10.,4.42));
#9945=CARTESIAN_POINT('',(-19.,-10.,5.8));
#9946=CARTESIAN_POINT('',(-19.,-10.,5.9));
#9947=CARTESIAN_POINT('',(-19.,10.,4.42));
#9948=CARTESIAN_POINT('',(-19.,10.,5.8));
#9949=CARTESIAN_POINT('',(-19.,10.,5.9));
#9950=CARTESIAN_POINT('',(19.,-10.,4.42));
#9951=CARTESIAN_POINT('',(19.,-10.,5.8));
#9952=CARTESIAN_POINT('',(19.,-10.,5.9));
#9953=CARTESIAN_POINT('',(19.,10.,4.42));
#9954=CARTESIAN_POINT('',(19.,10.,5.8));
#9955=CARTESIAN_POINT('',(19.,10.,5.9));
#9956=CARTESIAN_POINT('',(-10.8,19.42,37.));
#9957=CARTESIAN_POINT('',(-10.8,20.8,37.));
#9958=CARTESIAN_POINT('',(-10.8,20.9,37.));
#9959=CARTESIAN_POINT('',(-9.2,19.42,37.));
#9960=CARTESIAN_POINT('',(-9.2,20.8,37.));
#9961=CARTESIAN_POINT('',(-9.2,20.9,37.));
#9962=CARTESIAN_POINT('',(9.2,19.42,37.));
#9963=CARTESIAN_POINT('',(9.2,20.8,37.));
#9964=CARTESIAN_POINT('',(9.2,20.9,37.));
#9965=CARTESIAN_POINT('',(10.8,19.42,37.));
#9966=CARTESIAN_POINT('',(10.8,20.8,37.));
#9967=CARTESIAN_POINT('',(10.8,20.9,37.));
#9968=CARTESIAN_POINT('',(-10.,22.5,40.6));
#9969=CARTESIAN_POINT('',(-10.,22.5,40.68));
#9970=CARTESIAN_POINT('',(10.,22.5,40.6));
#9971=CARTESIAN_POINT('',(10.,22.5,40.68));
#9972=UNCERTAINTY_MEASURE_WITH_UNIT(LENGTH_MEASURE(0.001),#10020,
'DISTANCE_ACCURACY_VALUE',
'Maximum model space distance between geometric entities at asserted c
onnectivities');
#9973=UNCERTAINTY_MEASURE_WITH_UNIT(LENGTH_MEASURE(0.001),#10020,
'DISTANCE_ACCURACY_VALUE',
'Maximum model space distance between geometric entities at asserted c
onnectivities');
#9974=UNCERTAINTY_MEASURE_WITH_UNIT(LENGTH_MEASURE(0.001),#10020,
'DISTANCE_ACCURACY_VALUE',
'Maximum model space distance between geometric entities at asserted c
onnectivities');
#9975=UNCERTAINTY_MEASURE_WITH_UNIT(LENGTH_MEASURE(0.001),#10020,
'DISTANCE_ACCURACY_VALUE',
'Maximum model space distance between geometric entities at asserted c
onnectivities');
#9976=UNCERTAINTY_MEASURE_WITH_UNIT(LENGTH_MEASURE(0.001),#10020,
'DISTANCE_ACCURACY_VALUE',
'Maximum model space distance between geometric entities at asserted c
onnectivities');
#9977=UNCERTAINTY_MEASURE_WITH_UNIT(LENGTH_MEASURE(0.001),#10020,
'DISTANCE_ACCURACY_VALUE',
'Maximum model space distance between geometric entities at asserted c
onnectivities');
#9978=UNCERTAINTY_MEASURE_WITH_UNIT(LENGTH_MEASURE(0.001),#10020,
'DISTANCE_ACCURACY_VALUE',
'Maximum model space distance between geometric entities at asserted c
onnectivities');
#9979=UNCERTAINTY_MEASURE_WITH_UNIT(LENGTH_MEASURE(0.001),#10020,
'DISTANCE_ACCURACY_VALUE',
'Maximum model space distance between geometric entities at asserted c
onnectivities');
#9980=UNCERTAINTY_MEASURE_WITH_UNIT(LENGTH_MEASURE(0.001),#10020,
'DISTANCE_ACCURACY_VALUE',
'Maximum model space distance between geometric entities at asserted c
onnectivities');
#9981=UNCERTAINTY_MEASURE_WITH_UNIT(LENGTH_MEASURE(0.001),#10020,
'DISTANCE_ACCURACY_VALUE',
'Maximum model space distance between geometric entities at asserted c
onnectivities');
#9982=UNCERTAINTY_MEASURE_WITH_UNIT(LENGTH_MEASURE(0.001),#10020,
'DISTANCE_ACCURACY_VALUE',
'Maximum model space distance between geometric entities at asserted c
onnectivities');
#9983=UNCERTAINTY_MEASURE_WITH_UNIT(LENGTH_MEASURE(0.001),#10020,
'DISTANCE_ACCURACY_VALUE',
'Maximum model space distance between geometric entities at asserted c
onnectivities');
#9984=UNCERTAINTY_MEASURE_WITH_UNIT(LENGTH_MEASURE(0.001),#10020,
'DISTANCE_ACCURACY_VALUE',
'Maximum model space distance between geometric entities at asserted c
onnectivities');
#9985=UNCERTAINTY_MEASURE_WITH_UNIT(LENGTH_MEASURE(0.001),#10020,
'DISTANCE_ACCURACY_VALUE',
'Maximum model space distance between geometric entities at asserted c
onnectivities');
#9986=UNCERTAINTY_MEASURE_WITH_UNIT(LENGTH_MEASURE(0.001),#10020,
'DISTANCE_ACCURACY_VALUE',
'Maximum model space distance between geometric entities at asserted c
onnectivities');
#9987=UNCERTAINTY_MEASURE_WITH_UNIT(LENGTH_MEASURE(0.001),#10020,
'DISTANCE_ACCURACY_VALUE',
'Maximum model space distance between geometric entities at asserted c
onnectivities');
#9988=UNCERTAINTY_MEASURE_WITH_UNIT(LENGTH_MEASURE(0.001),#10020,
'DISTANCE_ACCURACY_VALUE',
'Maximum model space distance between geometric entities at asserted c
onnectivities');
#9989=UNCERTAINTY_MEASURE_WITH_UNIT(LENGTH_MEASURE(0.001),#10020,
'DISTANCE_ACCURACY_VALUE',
'Maximum model space distance between geometric entities at asserted c
onnectivities');
#9990=UNCERTAINTY_MEASURE_WITH_UNIT(LENGTH_MEASURE(0.001),#10020,
'DISTANCE_ACCURACY_VALUE',
'Maximum model space distance between geometric entities at asserted c
onnectivities');
#9991=UNCERTAINTY_MEASURE_WITH_UNIT(LENGTH_MEASURE(0.001),#10020,
'DISTANCE_ACCURACY_VALUE',
'Maximum model space distance between geometric entities at asserted c
onnectivities');
#9992=UNCERTAINTY_MEASURE_WITH_UNIT(LENGTH_MEASURE(0.001),#10020,
'DISTANCE_ACCURACY_VALUE',
'Maximum model space distance between geometric entities at asserted c
onnectivities');
#9993=UNCERTAINTY_MEASURE_WITH_UNIT(LENGTH_MEASURE(0.001),#10020,
'DISTANCE_ACCURACY_VALUE',
'Maximum model space distance between geometric entities at asserted c
onnectivities');
#9994=UNCERTAINTY_MEASURE_WITH_UNIT(LENGTH_MEASURE(0.001),#10020,
'DISTANCE_ACCURACY_VALUE',
'Maximum model space distance between geometric entities at asserted c
onnectivities');
#9995=UNCERTAINTY_MEASURE_WITH_UNIT(LENGTH_MEASURE(0.001),#10020,
'DISTANCE_ACCURACY_VALUE',
'Maximum model space distance between geometric entities at asserted c
onnectivities');
#9996=(
GEOMETRIC_REPRESENTATION_CONTEXT(3)
GLOBAL_UNCERTAINTY_ASSIGNED_CONTEXT((#9972))
GLOBAL_UNIT_ASSIGNED_CONTEXT((#10020,#10022,#10023))
REPRESENTATION_CONTEXT('','3D')
);
#9997=(
GEOMETRIC_REPRESENTATION_CONTEXT(3)
GLOBAL_UNCERTAINTY_ASSIGNED_CONTEXT((#9973))
GLOBAL_UNIT_ASSIGNED_CONTEXT((#10020,#10022,#10023))
REPRESENTATION_CONTEXT('','3D')
);
#9998=(
GEOMETRIC_REPRESENTATION_CONTEXT(3)
GLOBAL_UNCERTAINTY_ASSIGNED_CONTEXT((#9974))
GLOBAL_UNIT_ASSIGNED_CONTEXT((#10020,#10022,#10023))
REPRESENTATION_CONTEXT('','3D')
);
#9999=(
GEOMETRIC_REPRESENTATION_CONTEXT(3)
GLOBAL_UNCERTAINTY_ASSIGNED_CONTEXT((#9975))
GLOBAL_UNIT_ASSIGNED_CONTEXT((#10020,#10022,#10023))
REPRESENTATION_CONTEXT('','3D')
);
#10000=(
GEOMETRIC_REPRESENTATION_CONTEXT(3)
GLOBAL_UNCERTAINTY_ASSIGNED_CONTEXT((#9976))
GLOBAL_UNIT_ASSIGNED_CONTEXT((#10020,#10022,#10023))
REPRESENTATION_CONTEXT('','3D')
);
#10001=(
GEOMETRIC_REPRESENTATION_CONTEXT(3)
GLOBAL_UNCERTAINTY_ASSIGNED_CONTEXT((#9977))
GLOBAL_UNIT_ASSIGNED_CONTEXT((#10020,#10022,#10023))
REPRESENTATION_CONTEXT('','3D')
);
#10002=(
GEOMETRIC_REPRESENTATION_CONTEXT(3)
GLOBAL_UNCERTAINTY_ASSIGNED_CONTEXT((#9978))
GLOBAL_UNIT_ASSIGNED_CONTEXT((#10020,#10022,#10023))
REPRESENTATION_CONTEXT('','3D')
);
#10003=(
GEOMETRIC_REPRESENTATION_CONTEXT(3)
GLOBAL_UNCERTAINTY_ASSIGNED_CONTEXT((#9979))
GLOBAL_UNIT_ASSIGNED_CONTEXT((#10020,#10022,#10023))
REPRESENTATION_CONTEXT('','3D')
);
#10004=(
GEOMETRIC_REPRESENTATION_CONTEXT(3)
GLOBAL_UNCERTAINTY_ASSIGNED_CONTEXT((#9980))
GLOBAL_UNIT_ASSIGNED_CONTEXT((#10020,#10022,#10023))
REPRESENTATION_CONTEXT('','3D')
);
#10005=(
GEOMETRIC_REPRESENTATION_CONTEXT(3)
GLOBAL_UNCERTAINTY_ASSIGNED_CONTEXT((#9981))
GLOBAL_UNIT_ASSIGNED_CONTEXT((#10020,#10022,#10023))
REPRESENTATION_CONTEXT('','3D')
);
#10006=(
GEOMETRIC_REPRESENTATION_CONTEXT(3)
GLOBAL_UNCERTAINTY_ASSIGNED_CONTEXT((#9982))
GLOBAL_UNIT_ASSIGNED_CONTEXT((#10020,#10022,#10023))
REPRESENTATION_CONTEXT('','3D')
);
#10007=(
GEOMETRIC_REPRESENTATION_CONTEXT(3)
GLOBAL_UNCERTAINTY_ASSIGNED_CONTEXT((#9983))
GLOBAL_UNIT_ASSIGNED_CONTEXT((#10020,#10022,#10023))
REPRESENTATION_CONTEXT('','3D')
);
#10008=(
GEOMETRIC_REPRESENTATION_CONTEXT(3)
GLOBAL_UNCERTAINTY_ASSIGNED_CONTEXT((#9984))
GLOBAL_UNIT_ASSIGNED_CONTEXT((#10020,#10022,#10023))
REPRESENTATION_CONTEXT('','3D')
);
#10009=(
GEOMETRIC_REPRESENTATION_CONTEXT(3)
GLOBAL_UNCERTAINTY_ASSIGNED_CONTEXT((#9985))
GLOBAL_UNIT_ASSIGNED_CONTEXT((#10020,#10022,#10023))
REPRESENTATION_CONTEXT('','3D')
);
#10010=(
GEOMETRIC_REPRESENTATION_CONTEXT(3)
GLOBAL_UNCERTAINTY_ASSIGNED_CONTEXT((#9986))
GLOBAL_UNIT_ASSIGNED_CONTEXT((#10020,#10022,#10023))
REPRESENTATION_CONTEXT('','3D')
);
#10011=(
GEOMETRIC_REPRESENTATION_CONTEXT(3)
GLOBAL_UNCERTAINTY_ASSIGNED_CONTEXT((#9987))
GLOBAL_UNIT_ASSIGNED_CONTEXT((#10020,#10022,#10023))
REPRESENTATION_CONTEXT('','3D')
);
#10012=(
GEOMETRIC_REPRESENTATION_CONTEXT(3)
GLOBAL_UNCERTAINTY_ASSIGNED_CONTEXT((#9988))
GLOBAL_UNIT_ASSIGNED_CONTEXT((#10020,#10022,#10023))
REPRESENTATION_CONTEXT('','3D')
);
#10013=(
GEOMETRIC_REPRESENTATION_CONTEXT(3)
GLOBAL_UNCERTAINTY_ASSIGNED_CONTEXT((#9989))
GLOBAL_UNIT_ASSIGNED_CONTEXT((#10020,#10022,#10023))
REPRESENTATION_CONTEXT('','3D')
);
#10014=(
GEOMETRIC_REPRESENTATION_CONTEXT(3)
GLOBAL_UNCERTAINTY_ASSIGNED_CONTEXT((#9990))
GLOBAL_UNIT_ASSIGNED_CONTEXT((#10020,#10022,#10023))
REPRESENTATION_CONTEXT('','3D')
);
#10015=(
GEOMETRIC_REPRESENTATION_CONTEXT(3)
GLOBAL_UNCERTAINTY_ASSIGNED_CONTEXT((#9991))
GLOBAL_UNIT_ASSIGNED_CONTEXT((#10020,#10022,#10023))
REPRESENTATION_CONTEXT('','3D')
);
#10016=(
GEOMETRIC_REPRESENTATION_CONTEXT(3)
GLOBAL_UNCERTAINTY_ASSIGNED_CONTEXT((#9992))
GLOBAL_UNIT_ASSIGNED_CONTEXT((#10020,#10022,#10023))
REPRESENTATION_CONTEXT('','3D')
);
#10017=(
GEOMETRIC_REPRESENTATION_CONTEXT(3)
GLOBAL_UNCERTAINTY_ASSIGNED_CONTEXT((#9993))
GLOBAL_UNIT_ASSIGNED_CONTEXT((#10020,#10022,#10023))
REPRESENTATION_CONTEXT('','3D')
);
#10018=(
GEOMETRIC_REPRESENTATION_CONTEXT(3)
GLOBAL_UNCERTAINTY_ASSIGNED_CONTEXT((#9994))
GLOBAL_UNIT_ASSIGNED_CONTEXT((#10020,#10022,#10023))
REPRESENTATION_CONTEXT('','3D')
);
#10019=(
GEOMETRIC_REPRESENTATION_CONTEXT(3)
GLOBAL_UNCERTAINTY_ASSIGNED_CONTEXT((#9995))
GLOBAL_UNIT_ASSIGNED_CONTEXT((#10020,#10022,#10023))
REPRESENTATION_CONTEXT('','3D')
);
#10020=(
LENGTH_UNIT()
NAMED_UNIT(*)
SI_UNIT(.CENTI.,.METRE.)
);
#10021=(
LENGTH_UNIT()
NAMED_UNIT(*)
SI_UNIT($,.METRE.)
);
#10022=(
NAMED_UNIT(*)
PLANE_ANGLE_UNIT()
SI_UNIT($,.RADIAN.)
);
#10023=(
NAMED_UNIT(*)
SI_UNIT($,.STERADIAN.)
SOLID_ANGLE_UNIT()
);
#10024=SHAPE_DEFINITION_REPRESENTATION(#10047,#10167);
#10025=SHAPE_DEFINITION_REPRESENTATION(#10048,#10168);
#10026=SHAPE_DEFINITION_REPRESENTATION(#10049,#10169);
#10027=SHAPE_DEFINITION_REPRESENTATION(#10050,#10170);
#10028=SHAPE_DEFINITION_REPRESENTATION(#10051,#10171);
#10029=SHAPE_DEFINITION_REPRESENTATION(#10052,#10172);
#10030=SHAPE_DEFINITION_REPRESENTATION(#10053,#10173);
#10031=SHAPE_DEFINITION_REPRESENTATION(#10054,#10174);
#10032=SHAPE_DEFINITION_REPRESENTATION(#10055,#10175);
#10033=SHAPE_DEFINITION_REPRESENTATION(#10056,#10176);
#10034=SHAPE_DEFINITION_REPRESENTATION(#10057,#10177);
#10035=SHAPE_DEFINITION_REPRESENTATION(#10058,#10178);
#10036=SHAPE_DEFINITION_REPRESENTATION(#10059,#10179);
#10037=SHAPE_DEFINITION_REPRESENTATION(#10060,#10180);
#10038=SHAPE_DEFINITION_REPRESENTATION(#10061,#10181);
#10039=SHAPE_DEFINITION_REPRESENTATION(#10062,#10182);
#10040=SHAPE_DEFINITION_REPRESENTATION(#10063,#10183);
#10041=SHAPE_DEFINITION_REPRESENTATION(#10064,#10184);
#10042=SHAPE_DEFINITION_REPRESENTATION(#10065,#10185);
#10043=SHAPE_DEFINITION_REPRESENTATION(#10066,#10186);
#10044=SHAPE_DEFINITION_REPRESENTATION(#10067,#10187);
#10045=SHAPE_DEFINITION_REPRESENTATION(#10068,#10188);
#10046=SHAPE_DEFINITION_REPRESENTATION(#10069,#10189);
#10047=PRODUCT_DEFINITION_SHAPE('',$,#10191);
#10048=PRODUCT_DEFINITION_SHAPE('',$,#10192);
#10049=PRODUCT_DEFINITION_SHAPE('',$,#10193);
#10050=PRODUCT_DEFINITION_SHAPE('',$,#10194);
#10051=PRODUCT_DEFINITION_SHAPE('',$,#10195);
#10052=PRODUCT_DEFINITION_SHAPE('',$,#10196);
#10053=PRODUCT_DEFINITION_SHAPE('',$,#10197);
#10054=PRODUCT_DEFINITION_SHAPE('',$,#10198);
#10055=PRODUCT_DEFINITION_SHAPE('',$,#10199);
#10056=PRODUCT_DEFINITION_SHAPE('',$,#10200);
#10057=PRODUCT_DEFINITION_SHAPE('',$,#10201);
#10058=PRODUCT_DEFINITION_SHAPE('',$,#10202);
#10059=PRODUCT_DEFINITION_SHAPE('',$,#10203);
#10060=PRODUCT_DEFINITION_SHAPE('',$,#10204);
#10061=PRODUCT_DEFINITION_SHAPE('',$,#10205);
#10062=PRODUCT_DEFINITION_SHAPE('',$,#10206);
#10063=PRODUCT_DEFINITION_SHAPE('',$,#10207);
#10064=PRODUCT_DEFINITION_SHAPE('',$,#10208);
#10065=PRODUCT_DEFINITION_SHAPE('',$,#10209);
#10066=PRODUCT_DEFINITION_SHAPE('',$,#10210);
#10067=PRODUCT_DEFINITION_SHAPE('',$,#10211);
#10068=PRODUCT_DEFINITION_SHAPE('',$,#10212);
#10069=PRODUCT_DEFINITION_SHAPE('',$,#10213);
#10070=PRODUCT_DEFINITION_SHAPE($,$,#302);
#10071=PRODUCT_DEFINITION_SHAPE($,$,#303);
#10072=PRODUCT_DEFINITION_SHAPE($,$,#304);
#10073=PRODUCT_DEFINITION_SHAPE($,$,#305);
#10074=PRODUCT_DEFINITION_SHAPE($,$,#306);
#10075=PRODUCT_DEFINITION_SHAPE($,$,#307);
#10076=PRODUCT_DEFINITION_SHAPE($,$,#308);
#10077=PRODUCT_DEFINITION_SHAPE($,$,#309);
#10078=PRODUCT_DEFINITION_SHAPE($,$,#310);
#10079=PRODUCT_DEFINITION_SHAPE($,$,#311);
#10080=PRODUCT_DEFINITION_SHAPE($,$,#312);
#10081=PRODUCT_DEFINITION_SHAPE($,$,#313);
#10082=PRODUCT_DEFINITION_SHAPE($,$,#314);
#10083=PRODUCT_DEFINITION_SHAPE($,$,#315);
#10084=PRODUCT_DEFINITION_SHAPE($,$,#316);
#10085=PRODUCT_DEFINITION_SHAPE($,$,#317);
#10086=PRODUCT_DEFINITION_SHAPE($,$,#318);
#10087=PRODUCT_DEFINITION_SHAPE($,$,#319);
#10088=PRODUCT_DEFINITION_SHAPE($,$,#320);
#10089=PRODUCT_DEFINITION_SHAPE($,$,#321);
#10090=PRODUCT_DEFINITION_SHAPE($,$,#322);
#10091=PRODUCT_DEFINITION_SHAPE($,$,#323);
#10092=PRODUCT_DEFINITION_SHAPE($,$,#324);
#10093=PRODUCT_DEFINITION_SHAPE($,$,#325);
#10094=PRODUCT_DEFINITION_SHAPE($,$,#326);
#10095=PRODUCT_DEFINITION_SHAPE($,$,#327);
#10096=PRODUCT_DEFINITION_SHAPE($,$,#328);
#10097=PRODUCT_DEFINITION_SHAPE($,$,#329);
#10098=PRODUCT_DEFINITION_SHAPE($,$,#330);
#10099=PRODUCT_DEFINITION_SHAPE($,$,#331);
#10100=PRODUCT_DEFINITION_SHAPE($,$,#332);
#10101=PRODUCT_DEFINITION_SHAPE($,$,#333);
#10102=PRODUCT_DEFINITION_SHAPE($,$,#334);
#10103=PRODUCT_DEFINITION_SHAPE($,$,#335);
#10104=PRODUCT_DEFINITION_SHAPE($,$,#336);
#10105=PRODUCT_DEFINITION_SHAPE($,$,#337);
#10106=PRODUCT_DEFINITION_SHAPE($,$,#338);
#10107=PRODUCT_DEFINITION_SHAPE($,$,#339);
#10108=PRODUCT_DEFINITION_SHAPE($,$,#340);
#10109=PRODUCT_DEFINITION_SHAPE($,$,#341);
#10110=PRODUCT_DEFINITION_SHAPE($,$,#342);
#10111=PRODUCT_DEFINITION_SHAPE($,$,#343);
#10112=PRODUCT_DEFINITION_SHAPE($,$,#344);
#10113=PRODUCT_DEFINITION_SHAPE($,$,#345);
#10114=PRODUCT_DEFINITION_SHAPE($,$,#346);
#10115=PRODUCT_DEFINITION_SHAPE($,$,#347);
#10116=PRODUCT_DEFINITION_SHAPE($,$,#348);
#10117=PRODUCT_DEFINITION_SHAPE($,$,#349);
#10118=PRODUCT_DEFINITION_SHAPE($,$,#350);
#10119=PRODUCT_DEFINITION_SHAPE($,$,#351);
#10120=PRODUCT_DEFINITION_SHAPE($,$,#352);
#10121=PRODUCT_DEFINITION_SHAPE($,$,#353);
#10122=PRODUCT_DEFINITION_SHAPE($,$,#354);
#10123=PRODUCT_DEFINITION_SHAPE($,$,#355);
#10124=PRODUCT_DEFINITION_SHAPE($,$,#356);
#10125=PRODUCT_DEFINITION_SHAPE($,$,#357);
#10126=PRODUCT_DEFINITION_SHAPE($,$,#358);
#10127=PRODUCT_DEFINITION_SHAPE($,$,#359);
#10128=PRODUCT_DEFINITION_SHAPE($,$,#360);
#10129=PRODUCT_DEFINITION_SHAPE($,$,#361);
#10130=PRODUCT_DEFINITION_SHAPE($,$,#362);
#10131=PRODUCT_DEFINITION_SHAPE($,$,#363);
#10132=PRODUCT_DEFINITION_SHAPE($,$,#364);
#10133=PRODUCT_DEFINITION_SHAPE($,$,#365);
#10134=PRODUCT_DEFINITION_SHAPE($,$,#366);
#10135=PRODUCT_DEFINITION_SHAPE($,$,#367);
#10136=PRODUCT_DEFINITION_SHAPE($,$,#368);
#10137=PRODUCT_DEFINITION_SHAPE($,$,#369);
#10138=PRODUCT_DEFINITION_SHAPE($,$,#370);
#10139=PRODUCT_DEFINITION_SHAPE($,$,#371);
#10140=PRODUCT_DEFINITION_SHAPE($,$,#372);
#10141=PRODUCT_DEFINITION_SHAPE($,$,#373);
#10142=PRODUCT_DEFINITION_SHAPE($,$,#374);
#10143=PRODUCT_DEFINITION_SHAPE($,$,#375);
#10144=PRODUCT_DEFINITION_SHAPE($,$,#376);
#10145=PRODUCT_DEFINITION_SHAPE($,$,#377);
#10146=PRODUCT_DEFINITION_SHAPE($,$,#378);
#10147=PRODUCT_DEFINITION_SHAPE($,$,#379);
#10148=PRODUCT_DEFINITION_SHAPE($,$,#380);
#10149=PRODUCT_DEFINITION_SHAPE($,$,#381);
#10150=PRODUCT_DEFINITION_SHAPE($,$,#382);
#10151=PRODUCT_DEFINITION_SHAPE($,$,#383);
#10152=PRODUCT_DEFINITION_SHAPE($,$,#384);
#10153=PRODUCT_DEFINITION_SHAPE($,$,#385);
#10154=PRODUCT_DEFINITION_SHAPE($,$,#386);
#10155=PRODUCT_DEFINITION_SHAPE($,$,#387);
#10156=PRODUCT_DEFINITION_SHAPE($,$,#388);
#10157=PRODUCT_DEFINITION_SHAPE($,$,#389);
#10158=PRODUCT_DEFINITION_SHAPE($,$,#390);
#10159=PRODUCT_DEFINITION_SHAPE($,$,#391);
#10160=PRODUCT_DEFINITION_SHAPE($,$,#392);
#10161=PRODUCT_DEFINITION_SHAPE($,$,#393);
#10162=PRODUCT_DEFINITION_SHAPE($,$,#394);
#10163=PRODUCT_DEFINITION_SHAPE($,$,#395);
#10164=PRODUCT_DEFINITION_SHAPE($,$,#396);
#10165=PRODUCT_DEFINITION_SHAPE($,$,#397);
#10166=PRODUCT_DEFINITION_SHAPE($,$,#398);
#10167=SHAPE_REPRESENTATION('',(#5882,#6329,#6330,#6331,#6332,#6333,#6334,
#6335,#6336,#6337,#6338,#6339,#6340,#6341,#6342,#6343,#6344,#6345,#6346,
#6347,#6348,#6349,#6350,#6351,#6352,#6353,#6354,#6355,#6356,#6357,#6358,
#6359,#6360,#6361,#6362,#6363,#6364,#6365,#6366,#6367,#6368,#6369,#6370,
#6371,#6372,#6373,#6374,#6375,#6376,#6377,#6378,#6379,#6380,#6381,#6382,
#6383,#6384,#6385,#6386,#6387,#6388,#6389,#6390,#6391,#6392,#6393,#6394,
#6395,#6396,#6397,#6398,#6399,#6400,#6401,#6402,#6403,#6404,#6405,#6406,
#6407,#6408,#6409,#6410,#6411,#6412,#6413,#6414,#6415,#6416,#6417,#6418,
#6419,#6420,#6421,#6422,#6423,#6424,#6425),#9996);
#10168=SHAPE_REPRESENTATION('',(#5883),#9997);
#10169=SHAPE_REPRESENTATION('',(#5892),#9998);
#10170=SHAPE_REPRESENTATION('',(#5901),#9999);
#10171=SHAPE_REPRESENTATION('',(#5910),#10000);
#10172=SHAPE_REPRESENTATION('',(#5919),#10001);
#10173=SHAPE_REPRESENTATION('',(#5928),#10002);
#10174=SHAPE_REPRESENTATION('',(#5937),#10003);
#10175=SHAPE_REPRESENTATION('',(#5946),#10004);
#10176=SHAPE_REPRESENTATION('',(#5955),#10005);
#10177=SHAPE_REPRESENTATION('',(#5990),#10006);
#10178=SHAPE_REPRESENTATION('',(#6017),#10007);
#10179=SHAPE_REPRESENTATION('',(#6035),#10008);
#10180=SHAPE_REPRESENTATION('',(#6053),#10009);
#10181=SHAPE_REPRESENTATION('',(#6066),#10010);
#10182=SHAPE_REPRESENTATION('',(#6132),#10011);
#10183=SHAPE_REPRESENTATION('',(#6182),#10012);
#10184=SHAPE_REPRESENTATION('',(#6210),#10013);
#10185=SHAPE_REPRESENTATION('',(#6236),#10014);
#10186=SHAPE_REPRESENTATION('',(#6257),#10015);
#10187=SHAPE_REPRESENTATION('',(#6268),#10016);
#10188=SHAPE_REPRESENTATION('',(#6292),#10017);
#10189=SHAPE_REPRESENTATION('',(#6303),#10018);
#10190=PRODUCT_DEFINITION_CONTEXT('part definition',#10261,'design');
#10191=PRODUCT_DEFINITION('PAT-122','PAT-122',#10214,
#10190);
#10192=PRODUCT_DEFINITION('Foot','Foot',#10215,#10190);
#10193=PRODUCT_DEFINITION('Bonded foot pad','Bonded foot pad',
#10216,#10190);
#10194=PRODUCT_DEFINITION('Foot (1)','Foot (1)',#10217,#10190);
#10195=PRODUCT_DEFINITION('Bonded foot pad (1)',
'Bonded foot pad (1)',#10218,#10190);
#10196=PRODUCT_DEFINITION('Foot (2)','Foot (2)',#10219,
#10190);
#10197=PRODUCT_DEFINITION('Bonded foot pad (2)',
'Bonded foot pad (2)',#10220,#10190);
#10198=PRODUCT_DEFINITION('Foot (3)','Foot (3)',#10221,
#10190);
#10199=PRODUCT_DEFINITION('Bonded foot pad (3)',
'Bonded foot pad (3)',#10222,#10190);
#10200=PRODUCT_DEFINITION('Worktop','Worktop',#10223,#10190);
#10201=PRODUCT_DEFINITION('Lower shelf','Lower shelf',#10224,
#10190);
#10202=PRODUCT_DEFINITION('Accessory bracket',
'Accessory bracket',#10225,#10190);
#10203=PRODUCT_DEFINITION('Accessory bracket (1)',
'Accessory bracket (1)',#10226,#10190);
#10204=PRODUCT_DEFINITION('Accessory rail','Accessory rail',
#10227,#10190);
#10205=PRODUCT_DEFINITION('Slotted Extrusion - 20 x 20 x 400 mm',
'Slotted Extrusion - 20 x 20 x 400 mm',#10228,#10190);
#10206=PRODUCT_DEFINITION('360 mm cross member',
'360 mm cross member',#10229,#10190);
#10207=PRODUCT_DEFINITION('M5x30 frame screw',
'M5x30 frame screw',#10230,#10190);
#10208=PRODUCT_DEFINITION('Cap Screw - M5x20','Cap Screw - M5x20',
#10231,#10190);
#10209=PRODUCT_DEFINITION('Captive slot nut','Captive slot nut',
#10232,#10190);
#10210=PRODUCT_DEFINITION('Flat Washer - M5',
'Flat Washer - M5',#10233,#10190);
#10211=PRODUCT_DEFINITION('M5x14 Cap Screw','M5x14 Cap Screw',
#10234,#10190);
#10212=PRODUCT_DEFINITION('Flat Washer - M4',
'Flat Washer - M4',#10235,#10190);
#10213=PRODUCT_DEFINITION('Cap Screw - M4x16',
'Cap Screw - M4x16',#10236,#10190);
#10214=PRODUCT_DEFINITION_FORMATION('',$,#10263);
#10215=PRODUCT_DEFINITION_FORMATION('',$,#10264);
#10216=PRODUCT_DEFINITION_FORMATION('',$,#10265);
#10217=PRODUCT_DEFINITION_FORMATION('',$,#10266);
#10218=PRODUCT_DEFINITION_FORMATION('',$,#10267);
#10219=PRODUCT_DEFINITION_FORMATION('',$,#10268);
#10220=PRODUCT_DEFINITION_FORMATION('',$,#10269);
#10221=PRODUCT_DEFINITION_FORMATION('',$,#10270);
#10222=PRODUCT_DEFINITION_FORMATION('',$,#10271);
#10223=PRODUCT_DEFINITION_FORMATION('',$,#10272);
#10224=PRODUCT_DEFINITION_FORMATION('',$,#10273);
#10225=PRODUCT_DEFINITION_FORMATION('',$,#10274);
#10226=PRODUCT_DEFINITION_FORMATION('',$,#10275);
#10227=PRODUCT_DEFINITION_FORMATION('',$,#10276);
#10228=PRODUCT_DEFINITION_FORMATION('',$,#10277);
#10229=PRODUCT_DEFINITION_FORMATION('',$,#10278);
#10230=PRODUCT_DEFINITION_FORMATION('',$,#10279);
#10231=PRODUCT_DEFINITION_FORMATION('',$,#10280);
#10232=PRODUCT_DEFINITION_FORMATION('',$,#10281);
#10233=PRODUCT_DEFINITION_FORMATION('',$,#10282);
#10234=PRODUCT_DEFINITION_FORMATION('',$,#10283);
#10235=PRODUCT_DEFINITION_FORMATION('',$,#10284);
#10236=PRODUCT_DEFINITION_FORMATION('',$,#10285);
#10237=PRODUCT_RELATED_PRODUCT_CATEGORY('PAT-122','PAT-122',(#10263));
#10238=PRODUCT_RELATED_PRODUCT_CATEGORY('Foot','Foot',(#10264));
#10239=PRODUCT_RELATED_PRODUCT_CATEGORY('Bonded foot pad',
'Bonded foot pad',(#10265));
#10240=PRODUCT_RELATED_PRODUCT_CATEGORY('Foot (1)','Foot (1)',(#10266));
#10241=PRODUCT_RELATED_PRODUCT_CATEGORY('Bonded foot pad (1)',
'Bonded foot pad (1)',(#10267));
#10242=PRODUCT_RELATED_PRODUCT_CATEGORY('Foot (2)','Foot (2)',(#10268));
#10243=PRODUCT_RELATED_PRODUCT_CATEGORY('Bonded foot pad (2)',
'Bonded foot pad (2)',(#10269));
#10244=PRODUCT_RELATED_PRODUCT_CATEGORY('Foot (3)','Foot (3)',(#10270));
#10245=PRODUCT_RELATED_PRODUCT_CATEGORY('Bonded foot pad (3)',
'Bonded foot pad (3)',(#10271));
#10246=PRODUCT_RELATED_PRODUCT_CATEGORY('Worktop','Worktop',(#10272));
#10247=PRODUCT_RELATED_PRODUCT_CATEGORY('Lower shelf','Lower shelf',(#10273));
#10248=PRODUCT_RELATED_PRODUCT_CATEGORY('Accessory bracket',
'Accessory bracket',(#10274));
#10249=PRODUCT_RELATED_PRODUCT_CATEGORY('Accessory bracket (1)',
'Accessory bracket (1)',(#10275));
#10250=PRODUCT_RELATED_PRODUCT_CATEGORY('Accessory rail',
'Accessory rail',(#10276));
#10251=PRODUCT_RELATED_PRODUCT_CATEGORY(
'Slotted Extrusion - 20 x 20 x 400 mm',
'Slotted Extrusion - 20 x 20 x 400 mm',(#10277));
#10252=PRODUCT_RELATED_PRODUCT_CATEGORY('360 mm cross member',
'360 mm cross member',(#10278));
#10253=PRODUCT_RELATED_PRODUCT_CATEGORY('M5x30 frame screw',
'M5x30 frame screw',(#10279));
#10254=PRODUCT_RELATED_PRODUCT_CATEGORY('Cap Screw - M5x20',
'Cap Screw - M5x20',(#10280));
#10255=PRODUCT_RELATED_PRODUCT_CATEGORY('Captive slot nut',
'Captive slot nut',(#10281));
#10256=PRODUCT_RELATED_PRODUCT_CATEGORY('Flat Washer - M5',
'Flat Washer - M5',(#10282));
#10257=PRODUCT_RELATED_PRODUCT_CATEGORY('M5x14 Cap Screw',
'M5x14 Cap Screw',(#10283));
#10258=PRODUCT_RELATED_PRODUCT_CATEGORY('Flat Washer - M4',
'Flat Washer - M4',(#10284));
#10259=PRODUCT_RELATED_PRODUCT_CATEGORY('Cap Screw - M4x16',
'Cap Screw - M4x16',(#10285));
#10260=APPLICATION_PROTOCOL_DEFINITION('international standard',
'automotive_design',2009,#10261);
#10261=APPLICATION_CONTEXT(
'Core Data for Automotive Mechanical Design Process');
#10262=PRODUCT_CONTEXT('part definition',#10261,'mechanical');
#10263=PRODUCT('PAT-122','PAT-122','PAT-122',(#10262));
#10264=PRODUCT('Foot','Foot','Foot',(#10262));
#10265=PRODUCT('Bonded foot pad','Bonded foot pad',
'Bonded foot pad',(#10262));
#10266=PRODUCT('Foot (1)','Foot (1)','Foot (1)',(#10262));
#10267=PRODUCT('Bonded foot pad (1)','Bonded foot pad (1)',
'Bonded foot pad (1)',(#10262));
#10268=PRODUCT('Foot (2)','Foot (2)','Foot (2)',(#10262));
#10269=PRODUCT('Bonded foot pad (2)','Bonded foot pad (2)',
'Bonded foot pad (2)',(#10262));
#10270=PRODUCT('Foot (3)','Foot (3)','Foot (3)',(#10262));
#10271=PRODUCT('Bonded foot pad (3)','Bonded foot pad (3)',
'Bonded foot pad (3)',(#10262));
#10272=PRODUCT('Worktop','Worktop','Worktop',(#10262));
#10273=PRODUCT('Lower shelf','Lower shelf','Lower shelf',(#10262));
#10274=PRODUCT('Accessory bracket','Accessory bracket',
'Accessory bracket',(#10262));
#10275=PRODUCT('Accessory bracket (1)','Accessory bracket (1)',
'Accessory bracket (1)',(#10262));
#10276=PRODUCT('Accessory rail','Accessory rail',
'Accessory rail',(#10262));
#10277=PRODUCT('Slotted Extrusion - 20 x 20 x 400 mm',
'Slotted Extrusion - 20 x 20 x 400 mm',
'Slotted Extrusion - 20 x 20 x 400 mm',(#10262));
#10278=PRODUCT('360 mm cross member','360 mm cross member',
'360 mm cross member',(#10262));
#10279=PRODUCT('M5x30 frame screw','M5x30 frame screw',
'M5x30 frame screw',(#10262));
#10280=PRODUCT('Cap Screw - M5x20','Cap Screw - M5x20',
'Cap Screw - M5x20',(#10262));
#10281=PRODUCT('Captive slot nut','Captive slot nut',
'Captive slot nut',(#10262));
#10282=PRODUCT('Flat Washer - M5','Flat Washer - M5',
'Flat Washer - M5',(#10262));
#10283=PRODUCT('M5x14 Cap Screw','M5x14 Cap Screw',
'M5x14 Cap Screw',(#10262));
#10284=PRODUCT('Flat Washer - M4','Flat Washer - M4',
'Flat Washer - M4',(#10262));
#10285=PRODUCT('Cap Screw - M4x16','Cap Screw - M4x16',
'Cap Screw - M4x16',(#10262));
#10286=PRESENTATION_STYLE_ASSIGNMENT((#10291));
#10287=PRESENTATION_STYLE_ASSIGNMENT((#10292));
#10288=PRESENTATION_STYLE_ASSIGNMENT((#10293));
#10289=PRESENTATION_STYLE_ASSIGNMENT((#10294));
#10290=PRESENTATION_STYLE_ASSIGNMENT((#10295));
#10291=SURFACE_STYLE_USAGE(.BOTH.,#10296);
#10292=SURFACE_STYLE_USAGE(.BOTH.,#10297);
#10293=SURFACE_STYLE_USAGE(.BOTH.,#10298);
#10294=SURFACE_STYLE_USAGE(.BOTH.,#10299);
#10295=SURFACE_STYLE_USAGE(.BOTH.,#10300);
#10296=SURFACE_SIDE_STYLE('',(#10301));
#10297=SURFACE_SIDE_STYLE('',(#10302));
#10298=SURFACE_SIDE_STYLE('',(#10303));
#10299=SURFACE_SIDE_STYLE('',(#10304));
#10300=SURFACE_SIDE_STYLE('',(#10305));
#10301=SURFACE_STYLE_FILL_AREA(#10306);
#10302=SURFACE_STYLE_FILL_AREA(#10307);
#10303=SURFACE_STYLE_FILL_AREA(#10308);
#10304=SURFACE_STYLE_FILL_AREA(#10309);
#10305=SURFACE_STYLE_FILL_AREA(#10310);
#10306=FILL_AREA_STYLE('Steel - Satin',(#10311));
#10307=FILL_AREA_STYLE('CAD Library Painted - Deep blue',(#10312));
#10308=FILL_AREA_STYLE('CAD Library Painted - Graphite',(#10313));
#10309=FILL_AREA_STYLE('CAD Library Painted - Engineering blue',(#10314));
#10310=FILL_AREA_STYLE('CAD Library Painted - Steel gray',(#10315));
#10311=FILL_AREA_STYLE_COLOUR('Steel - Satin',#10316);
#10312=FILL_AREA_STYLE_COLOUR('CAD Library Painted - Deep blue',#10317);
#10313=FILL_AREA_STYLE_COLOUR('CAD Library Painted - Graphite',#10318);
#10314=FILL_AREA_STYLE_COLOUR('CAD Library Painted - Engineering blue',
#10319);
#10315=FILL_AREA_STYLE_COLOUR('CAD Library Painted - Steel gray',#10320);
#10316=COLOUR_RGB('Steel - Satin',0.627450980392157,0.627450980392157,0.627450980392157);
#10317=COLOUR_RGB('CAD Library Painted - Deep blue',0.0784313725490196,
0.203921568627451,0.349019607843137);
#10318=COLOUR_RGB('CAD Library Painted - Graphite',0.168627450980392,0.192156862745098,
0.231372549019608);
#10319=COLOUR_RGB('CAD Library Painted - Engineering blue',0.12156862745098,
0.356862745098039,0.6);
#10320=COLOUR_RGB('CAD Library Painted - Steel gray',0.592156862745098,
0.631372549019608,0.67843137254902);
#10321=COLOUR_RGB('Dark Blue',0.08,0.2,0.34);
#10322=FILL_AREA_STYLE_COLOUR('',#10321);
#10323=FILL_AREA_STYLE('',(#10322));
#10324=SURFACE_STYLE_FILL_AREA(#10323);
#10325=SURFACE_SIDE_STYLE('',(#10324));
#10326=SURFACE_STYLE_USAGE(.BOTH.,#10325);
#10327=PRESENTATION_STYLE_ASSIGNMENT((#10326));
#10328=COLOUR_RGB('Light Blue',0.38,0.62,0.78);
#10329=FILL_AREA_STYLE_COLOUR('',#10328);
#10330=FILL_AREA_STYLE('',(#10329));
#10331=SURFACE_STYLE_FILL_AREA(#10330);
#10332=SURFACE_SIDE_STYLE('',(#10331));
#10333=SURFACE_STYLE_USAGE(.BOTH.,#10332);
#10334=PRESENTATION_STYLE_ASSIGNMENT((#10333));
#10335=COLOUR_RGB('Sky Blue',0.24,0.69,0.87);
#10336=FILL_AREA_STYLE_COLOUR('',#10335);
#10337=FILL_AREA_STYLE('',(#10336));
#10338=SURFACE_STYLE_FILL_AREA(#10337);
#10339=SURFACE_SIDE_STYLE('',(#10338));
#10340=SURFACE_STYLE_USAGE(.BOTH.,#10339);
#10341=PRESENTATION_STYLE_ASSIGNMENT((#10340));
#10342=COLOUR_RGB('Grey',0.48,0.52,0.57);
#10343=FILL_AREA_STYLE_COLOUR('',#10342);
#10344=FILL_AREA_STYLE('',(#10343));
#10345=SURFACE_STYLE_FILL_AREA(#10344);
#10346=SURFACE_SIDE_STYLE('',(#10345));
#10347=SURFACE_STYLE_USAGE(.BOTH.,#10346);
#10348=PRESENTATION_STYLE_ASSIGNMENT((#10347));
#10349=COLOUR_RGB('Black',0.12,0.14,0.17);
#10350=FILL_AREA_STYLE_COLOUR('',#10349);
#10351=FILL_AREA_STYLE('',(#10350));
#10352=SURFACE_STYLE_FILL_AREA(#10351);
#10353=SURFACE_SIDE_STYLE('',(#10352));
#10354=SURFACE_STYLE_USAGE(.BOTH.,#10353);
#10355=PRESENTATION_STYLE_ASSIGNMENT((#10354));
#10356=COLOUR_RGB('Off White',0.89,0.88,0.83);
#10357=FILL_AREA_STYLE_COLOUR('',#10356);
#10358=FILL_AREA_STYLE('',(#10357));
#10359=SURFACE_STYLE_FILL_AREA(#10358);
#10360=SURFACE_SIDE_STYLE('',(#10359));
#10361=SURFACE_STYLE_USAGE(.BOTH.,#10360);
#10362=PRESENTATION_STYLE_ASSIGNMENT((#10361));
ENDSEC;
END-ISO-10303-21;
